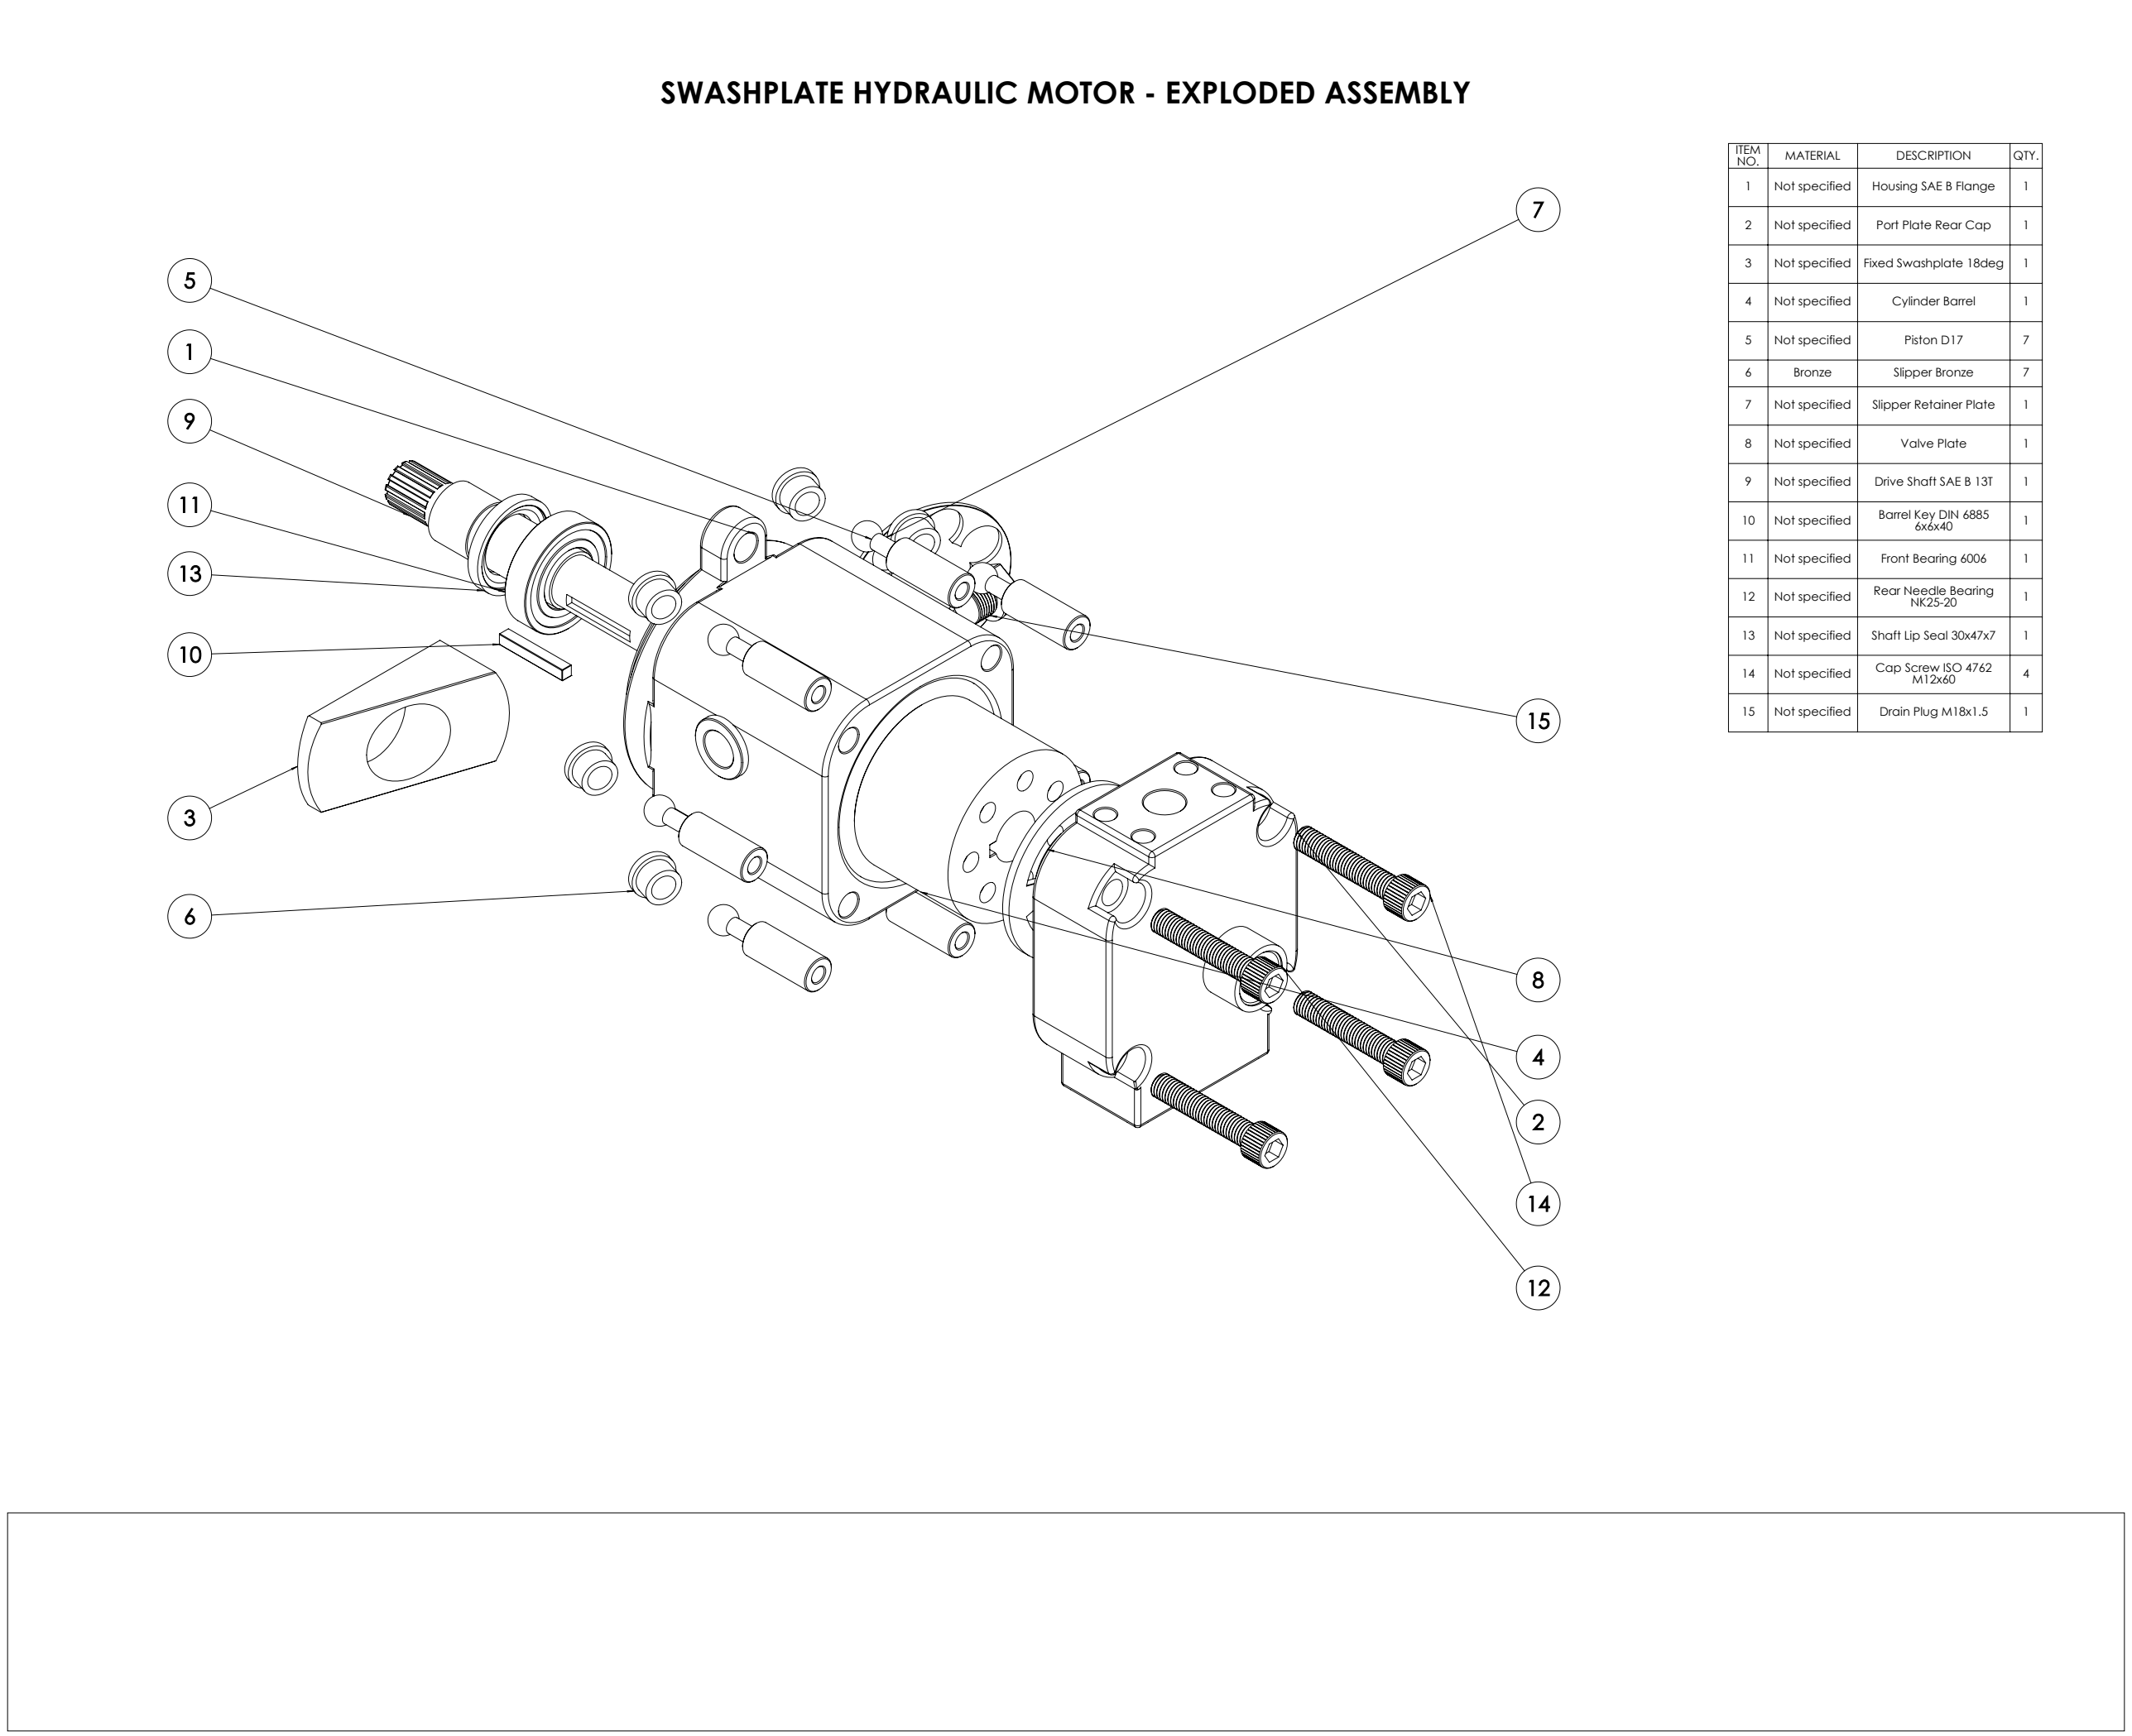
ISO-10303-21;
HEADER;
/* Generated by software containing ST-Developer
 * from STEP Tools, Inc. (www.steptools.com) 
 */

FILE_DESCRIPTION(
/* description */ (''),
/* implementation_level */ '2;1');

FILE_NAME(
/* name */ 'MAS-347',
/* time_stamp */ '2026-10-26T07:49:00-07:00',
/* author */ (''),
/* organization */ (''),
/* preprocessor_version */ 'ST-DEVELOPER v20.2',
/* originating_system */ 'Autodesk Translation Framework v15.15.0.0',
/* authorisation */ '');

FILE_SCHEMA (('AUTOMOTIVE_DESIGN { 1 0 10303 214 3 1 1 }'));
ENDSEC;

DATA;
#10=MECHANICAL_DESIGN_GEOMETRIC_PRESENTATION_REPRESENTATION('',(#177,#178,
#179,#180,#181,#182,#183,#184,#185,#186,#187,#188,#189,#190,#191),#38507);
#11=ITEM_DEFINED_TRANSFORMATION($,$,#15253,#16745);
#12=ITEM_DEFINED_TRANSFORMATION($,$,#15494,#16746);
#13=ITEM_DEFINED_TRANSFORMATION($,$,#15799,#16747);
#14=ITEM_DEFINED_TRANSFORMATION($,$,#15825,#16748);
#15=ITEM_DEFINED_TRANSFORMATION($,$,#15901,#16749);
#16=ITEM_DEFINED_TRANSFORMATION($,$,#15950,#16750);
#17=ITEM_DEFINED_TRANSFORMATION($,$,#16152,#16751);
#18=ITEM_DEFINED_TRANSFORMATION($,$,#16171,#16752);
#19=ITEM_DEFINED_TRANSFORMATION($,$,#16204,#16753);
#20=ITEM_DEFINED_TRANSFORMATION($,$,#16229,#16754);
#21=ITEM_DEFINED_TRANSFORMATION($,$,#16254,#16755);
#22=ITEM_DEFINED_TRANSFORMATION($,$,#16279,#16756);
#23=ITEM_DEFINED_TRANSFORMATION($,$,#16254,#16757);
#24=ITEM_DEFINED_TRANSFORMATION($,$,#16279,#16758);
#25=ITEM_DEFINED_TRANSFORMATION($,$,#16254,#16759);
#26=ITEM_DEFINED_TRANSFORMATION($,$,#16279,#16760);
#27=ITEM_DEFINED_TRANSFORMATION($,$,#16254,#16761);
#28=ITEM_DEFINED_TRANSFORMATION($,$,#16279,#16762);
#29=ITEM_DEFINED_TRANSFORMATION($,$,#16254,#16763);
#30=ITEM_DEFINED_TRANSFORMATION($,$,#16279,#16764);
#31=ITEM_DEFINED_TRANSFORMATION($,$,#16254,#16765);
#32=ITEM_DEFINED_TRANSFORMATION($,$,#16279,#16766);
#33=ITEM_DEFINED_TRANSFORMATION($,$,#16254,#16767);
#34=ITEM_DEFINED_TRANSFORMATION($,$,#16279,#16768);
#35=ITEM_DEFINED_TRANSFORMATION($,$,#16304,#16769);
#36=ITEM_DEFINED_TRANSFORMATION($,$,#16357,#16770);
#37=ITEM_DEFINED_TRANSFORMATION($,$,#16357,#16771);
#38=ITEM_DEFINED_TRANSFORMATION($,$,#16357,#16772);
#39=ITEM_DEFINED_TRANSFORMATION($,$,#16357,#16773);
#40=ITEM_DEFINED_TRANSFORMATION($,$,#16670,#16774);
#41=(
REPRESENTATION_RELATIONSHIP($,$,#38575,#38574)
REPRESENTATION_RELATIONSHIP_WITH_TRANSFORMATION(#11)
SHAPE_REPRESENTATION_RELATIONSHIP()
);
#42=(
REPRESENTATION_RELATIONSHIP($,$,#38576,#38574)
REPRESENTATION_RELATIONSHIP_WITH_TRANSFORMATION(#12)
SHAPE_REPRESENTATION_RELATIONSHIP()
);
#43=(
REPRESENTATION_RELATIONSHIP($,$,#38577,#38574)
REPRESENTATION_RELATIONSHIP_WITH_TRANSFORMATION(#13)
SHAPE_REPRESENTATION_RELATIONSHIP()
);
#44=(
REPRESENTATION_RELATIONSHIP($,$,#38578,#38574)
REPRESENTATION_RELATIONSHIP_WITH_TRANSFORMATION(#14)
SHAPE_REPRESENTATION_RELATIONSHIP()
);
#45=(
REPRESENTATION_RELATIONSHIP($,$,#38579,#38574)
REPRESENTATION_RELATIONSHIP_WITH_TRANSFORMATION(#15)
SHAPE_REPRESENTATION_RELATIONSHIP()
);
#46=(
REPRESENTATION_RELATIONSHIP($,$,#38580,#38574)
REPRESENTATION_RELATIONSHIP_WITH_TRANSFORMATION(#16)
SHAPE_REPRESENTATION_RELATIONSHIP()
);
#47=(
REPRESENTATION_RELATIONSHIP($,$,#38581,#38574)
REPRESENTATION_RELATIONSHIP_WITH_TRANSFORMATION(#17)
SHAPE_REPRESENTATION_RELATIONSHIP()
);
#48=(
REPRESENTATION_RELATIONSHIP($,$,#38582,#38574)
REPRESENTATION_RELATIONSHIP_WITH_TRANSFORMATION(#18)
SHAPE_REPRESENTATION_RELATIONSHIP()
);
#49=(
REPRESENTATION_RELATIONSHIP($,$,#38583,#38574)
REPRESENTATION_RELATIONSHIP_WITH_TRANSFORMATION(#19)
SHAPE_REPRESENTATION_RELATIONSHIP()
);
#50=(
REPRESENTATION_RELATIONSHIP($,$,#38584,#38574)
REPRESENTATION_RELATIONSHIP_WITH_TRANSFORMATION(#20)
SHAPE_REPRESENTATION_RELATIONSHIP()
);
#51=(
REPRESENTATION_RELATIONSHIP($,$,#38585,#38574)
REPRESENTATION_RELATIONSHIP_WITH_TRANSFORMATION(#21)
SHAPE_REPRESENTATION_RELATIONSHIP()
);
#52=(
REPRESENTATION_RELATIONSHIP($,$,#38586,#38574)
REPRESENTATION_RELATIONSHIP_WITH_TRANSFORMATION(#22)
SHAPE_REPRESENTATION_RELATIONSHIP()
);
#53=(
REPRESENTATION_RELATIONSHIP($,$,#38585,#38574)
REPRESENTATION_RELATIONSHIP_WITH_TRANSFORMATION(#23)
SHAPE_REPRESENTATION_RELATIONSHIP()
);
#54=(
REPRESENTATION_RELATIONSHIP($,$,#38586,#38574)
REPRESENTATION_RELATIONSHIP_WITH_TRANSFORMATION(#24)
SHAPE_REPRESENTATION_RELATIONSHIP()
);
#55=(
REPRESENTATION_RELATIONSHIP($,$,#38585,#38574)
REPRESENTATION_RELATIONSHIP_WITH_TRANSFORMATION(#25)
SHAPE_REPRESENTATION_RELATIONSHIP()
);
#56=(
REPRESENTATION_RELATIONSHIP($,$,#38586,#38574)
REPRESENTATION_RELATIONSHIP_WITH_TRANSFORMATION(#26)
SHAPE_REPRESENTATION_RELATIONSHIP()
);
#57=(
REPRESENTATION_RELATIONSHIP($,$,#38585,#38574)
REPRESENTATION_RELATIONSHIP_WITH_TRANSFORMATION(#27)
SHAPE_REPRESENTATION_RELATIONSHIP()
);
#58=(
REPRESENTATION_RELATIONSHIP($,$,#38586,#38574)
REPRESENTATION_RELATIONSHIP_WITH_TRANSFORMATION(#28)
SHAPE_REPRESENTATION_RELATIONSHIP()
);
#59=(
REPRESENTATION_RELATIONSHIP($,$,#38585,#38574)
REPRESENTATION_RELATIONSHIP_WITH_TRANSFORMATION(#29)
SHAPE_REPRESENTATION_RELATIONSHIP()
);
#60=(
REPRESENTATION_RELATIONSHIP($,$,#38586,#38574)
REPRESENTATION_RELATIONSHIP_WITH_TRANSFORMATION(#30)
SHAPE_REPRESENTATION_RELATIONSHIP()
);
#61=(
REPRESENTATION_RELATIONSHIP($,$,#38585,#38574)
REPRESENTATION_RELATIONSHIP_WITH_TRANSFORMATION(#31)
SHAPE_REPRESENTATION_RELATIONSHIP()
);
#62=(
REPRESENTATION_RELATIONSHIP($,$,#38586,#38574)
REPRESENTATION_RELATIONSHIP_WITH_TRANSFORMATION(#32)
SHAPE_REPRESENTATION_RELATIONSHIP()
);
#63=(
REPRESENTATION_RELATIONSHIP($,$,#38585,#38574)
REPRESENTATION_RELATIONSHIP_WITH_TRANSFORMATION(#33)
SHAPE_REPRESENTATION_RELATIONSHIP()
);
#64=(
REPRESENTATION_RELATIONSHIP($,$,#38586,#38574)
REPRESENTATION_RELATIONSHIP_WITH_TRANSFORMATION(#34)
SHAPE_REPRESENTATION_RELATIONSHIP()
);
#65=(
REPRESENTATION_RELATIONSHIP($,$,#38587,#38574)
REPRESENTATION_RELATIONSHIP_WITH_TRANSFORMATION(#35)
SHAPE_REPRESENTATION_RELATIONSHIP()
);
#66=(
REPRESENTATION_RELATIONSHIP($,$,#38588,#38574)
REPRESENTATION_RELATIONSHIP_WITH_TRANSFORMATION(#36)
SHAPE_REPRESENTATION_RELATIONSHIP()
);
#67=(
REPRESENTATION_RELATIONSHIP($,$,#38588,#38574)
REPRESENTATION_RELATIONSHIP_WITH_TRANSFORMATION(#37)
SHAPE_REPRESENTATION_RELATIONSHIP()
);
#68=(
REPRESENTATION_RELATIONSHIP($,$,#38588,#38574)
REPRESENTATION_RELATIONSHIP_WITH_TRANSFORMATION(#38)
SHAPE_REPRESENTATION_RELATIONSHIP()
);
#69=(
REPRESENTATION_RELATIONSHIP($,$,#38588,#38574)
REPRESENTATION_RELATIONSHIP_WITH_TRANSFORMATION(#39)
SHAPE_REPRESENTATION_RELATIONSHIP()
);
#70=(
REPRESENTATION_RELATIONSHIP($,$,#38589,#38574)
REPRESENTATION_RELATIONSHIP_WITH_TRANSFORMATION(#40)
SHAPE_REPRESENTATION_RELATIONSHIP()
);
#71=CONTEXT_DEPENDENT_SHAPE_REPRESENTATION(#41,#38544);
#72=CONTEXT_DEPENDENT_SHAPE_REPRESENTATION(#42,#38545);
#73=CONTEXT_DEPENDENT_SHAPE_REPRESENTATION(#43,#38546);
#74=CONTEXT_DEPENDENT_SHAPE_REPRESENTATION(#44,#38547);
#75=CONTEXT_DEPENDENT_SHAPE_REPRESENTATION(#45,#38548);
#76=CONTEXT_DEPENDENT_SHAPE_REPRESENTATION(#46,#38549);
#77=CONTEXT_DEPENDENT_SHAPE_REPRESENTATION(#47,#38550);
#78=CONTEXT_DEPENDENT_SHAPE_REPRESENTATION(#48,#38551);
#79=CONTEXT_DEPENDENT_SHAPE_REPRESENTATION(#49,#38552);
#80=CONTEXT_DEPENDENT_SHAPE_REPRESENTATION(#50,#38553);
#81=CONTEXT_DEPENDENT_SHAPE_REPRESENTATION(#51,#38554);
#82=CONTEXT_DEPENDENT_SHAPE_REPRESENTATION(#52,#38555);
#83=CONTEXT_DEPENDENT_SHAPE_REPRESENTATION(#53,#38556);
#84=CONTEXT_DEPENDENT_SHAPE_REPRESENTATION(#54,#38557);
#85=CONTEXT_DEPENDENT_SHAPE_REPRESENTATION(#55,#38558);
#86=CONTEXT_DEPENDENT_SHAPE_REPRESENTATION(#56,#38559);
#87=CONTEXT_DEPENDENT_SHAPE_REPRESENTATION(#57,#38560);
#88=CONTEXT_DEPENDENT_SHAPE_REPRESENTATION(#58,#38561);
#89=CONTEXT_DEPENDENT_SHAPE_REPRESENTATION(#59,#38562);
#90=CONTEXT_DEPENDENT_SHAPE_REPRESENTATION(#60,#38563);
#91=CONTEXT_DEPENDENT_SHAPE_REPRESENTATION(#61,#38564);
#92=CONTEXT_DEPENDENT_SHAPE_REPRESENTATION(#62,#38565);
#93=CONTEXT_DEPENDENT_SHAPE_REPRESENTATION(#63,#38566);
#94=CONTEXT_DEPENDENT_SHAPE_REPRESENTATION(#64,#38567);
#95=CONTEXT_DEPENDENT_SHAPE_REPRESENTATION(#65,#38568);
#96=CONTEXT_DEPENDENT_SHAPE_REPRESENTATION(#66,#38569);
#97=CONTEXT_DEPENDENT_SHAPE_REPRESENTATION(#67,#38570);
#98=CONTEXT_DEPENDENT_SHAPE_REPRESENTATION(#68,#38571);
#99=CONTEXT_DEPENDENT_SHAPE_REPRESENTATION(#69,#38572);
#100=CONTEXT_DEPENDENT_SHAPE_REPRESENTATION(#70,#38573);
#101=NEXT_ASSEMBLY_USAGE_OCCURRENCE('01_Housing_SAE_B_Flange:2',
'01_Housing_SAE_B_Flange:2','01_Housing_SAE_B_Flange:2',#38591,#38592,
'01_Housing_SAE_B_Flange:2');
#102=NEXT_ASSEMBLY_USAGE_OCCURRENCE('02_Port_Plate_Rear_Cap:2',
'02_Port_Plate_Rear_Cap:2','02_Port_Plate_Rear_Cap:2',#38591,#38593,
'02_Port_Plate_Rear_Cap:2');
#103=NEXT_ASSEMBLY_USAGE_OCCURRENCE('03_Fixed_Swashplate_18deg:2',
'03_Fixed_Swashplate_18deg:2','03_Fixed_Swashplate_18deg:2',#38591,#38594,
'03_Fixed_Swashplate_18deg:2');
#104=NEXT_ASSEMBLY_USAGE_OCCURRENCE('04_Cylinder_Barrel:2',
'04_Cylinder_Barrel:2','04_Cylinder_Barrel:2',#38591,#38595,
'04_Cylinder_Barrel:2');
#105=NEXT_ASSEMBLY_USAGE_OCCURRENCE('08_Valve_Plate:2',
'08_Valve_Plate:2','08_Valve_Plate:2',#38591,#38596,'08_Valve_Plate:2');
#106=NEXT_ASSEMBLY_USAGE_OCCURRENCE('09_Drive_Shaft_SAE_B_13T:2',
'09_Drive_Shaft_SAE_B_13T:2','09_Drive_Shaft_SAE_B_13T:2',#38591,#38597,
'09_Drive_Shaft_SAE_B_13T:2');
#107=NEXT_ASSEMBLY_USAGE_OCCURRENCE('10_Barrel_Key_DIN_6885_6x6x40:2',
'10_Barrel_Key_DIN_6885_6x6x40:2','10_Barrel_Key_DIN_6885_6x6x40:2',#38591,
#38598,'10_Barrel_Key_DIN_6885_6x6x40:2');
#108=NEXT_ASSEMBLY_USAGE_OCCURRENCE('11_Front_Bearing_6006:2',
'11_Front_Bearing_6006:2','11_Front_Bearing_6006:2',#38591,#38599,
'11_Front_Bearing_6006:2');
#109=NEXT_ASSEMBLY_USAGE_OCCURRENCE('12_Rear_Needle_Bearing_NK25-20:2',
'12_Rear_Needle_Bearing_NK25-20:2','12_Rear_Needle_Bearing_NK25-20:2',#38591,
#38600,'12_Rear_Needle_Bearing_NK25-20:2');
#110=NEXT_ASSEMBLY_USAGE_OCCURRENCE('13_Shaft_Lip_Seal_30x47x7:2',
'13_Shaft_Lip_Seal_30x47x7:2','13_Shaft_Lip_Seal_30x47x7:2',#38591,#38601,
'13_Shaft_Lip_Seal_30x47x7:2');
#111=NEXT_ASSEMBLY_USAGE_OCCURRENCE('05_Piston_D17:2','05_Piston_D17:2',
'05_Piston_D17:2',#38591,#38602,'05_Piston_D17:2');
#112=NEXT_ASSEMBLY_USAGE_OCCURRENCE('06_Slipper_Bronze:2',
'06_Slipper_Bronze:2','06_Slipper_Bronze:2',#38591,#38603,
'06_Slipper_Bronze:2');
#113=NEXT_ASSEMBLY_USAGE_OCCURRENCE('05_Piston_D17:3','05_Piston_D17:3',
'05_Piston_D17:3',#38591,#38602,'05_Piston_D17:3');
#114=NEXT_ASSEMBLY_USAGE_OCCURRENCE('06_Slipper_Bronze:3',
'06_Slipper_Bronze:3','06_Slipper_Bronze:3',#38591,#38603,
'06_Slipper_Bronze:3');
#115=NEXT_ASSEMBLY_USAGE_OCCURRENCE('05_Piston_D17:4','05_Piston_D17:4',
'05_Piston_D17:4',#38591,#38602,'05_Piston_D17:4');
#116=NEXT_ASSEMBLY_USAGE_OCCURRENCE('06_Slipper_Bronze:4',
'06_Slipper_Bronze:4','06_Slipper_Bronze:4',#38591,#38603,
'06_Slipper_Bronze:4');
#117=NEXT_ASSEMBLY_USAGE_OCCURRENCE('05_Piston_D17:5','05_Piston_D17:5',
'05_Piston_D17:5',#38591,#38602,'05_Piston_D17:5');
#118=NEXT_ASSEMBLY_USAGE_OCCURRENCE('06_Slipper_Bronze:5',
'06_Slipper_Bronze:5','06_Slipper_Bronze:5',#38591,#38603,
'06_Slipper_Bronze:5');
#119=NEXT_ASSEMBLY_USAGE_OCCURRENCE('05_Piston_D17:6','05_Piston_D17:6',
'05_Piston_D17:6',#38591,#38602,'05_Piston_D17:6');
#120=NEXT_ASSEMBLY_USAGE_OCCURRENCE('06_Slipper_Bronze:6',
'06_Slipper_Bronze:6','06_Slipper_Bronze:6',#38591,#38603,
'06_Slipper_Bronze:6');
#121=NEXT_ASSEMBLY_USAGE_OCCURRENCE('05_Piston_D17:7','05_Piston_D17:7',
'05_Piston_D17:7',#38591,#38602,'05_Piston_D17:7');
#122=NEXT_ASSEMBLY_USAGE_OCCURRENCE('06_Slipper_Bronze:7',
'06_Slipper_Bronze:7','06_Slipper_Bronze:7',#38591,#38603,
'06_Slipper_Bronze:7');
#123=NEXT_ASSEMBLY_USAGE_OCCURRENCE('05_Piston_D17:8','05_Piston_D17:8',
'05_Piston_D17:8',#38591,#38602,'05_Piston_D17:8');
#124=NEXT_ASSEMBLY_USAGE_OCCURRENCE('06_Slipper_Bronze:8',
'06_Slipper_Bronze:8','06_Slipper_Bronze:8',#38591,#38603,
'06_Slipper_Bronze:8');
#125=NEXT_ASSEMBLY_USAGE_OCCURRENCE('07_Slipper_Retainer_Plate:2',
'07_Slipper_Retainer_Plate:2','07_Slipper_Retainer_Plate:2',#38591,#38604,
'07_Slipper_Retainer_Plate:2');
#126=NEXT_ASSEMBLY_USAGE_OCCURRENCE('14_Cap_Screw_ISO_4762_M12x60:2',
'14_Cap_Screw_ISO_4762_M12x60:2','14_Cap_Screw_ISO_4762_M12x60:2',#38591,
#38605,'14_Cap_Screw_ISO_4762_M12x60:2');
#127=NEXT_ASSEMBLY_USAGE_OCCURRENCE('14_Cap_Screw_ISO_4762_M12x60:3',
'14_Cap_Screw_ISO_4762_M12x60:3','14_Cap_Screw_ISO_4762_M12x60:3',#38591,
#38605,'14_Cap_Screw_ISO_4762_M12x60:3');
#128=NEXT_ASSEMBLY_USAGE_OCCURRENCE('14_Cap_Screw_ISO_4762_M12x60:4',
'14_Cap_Screw_ISO_4762_M12x60:4','14_Cap_Screw_ISO_4762_M12x60:4',#38591,
#38605,'14_Cap_Screw_ISO_4762_M12x60:4');
#129=NEXT_ASSEMBLY_USAGE_OCCURRENCE('14_Cap_Screw_ISO_4762_M12x60:5',
'14_Cap_Screw_ISO_4762_M12x60:5','14_Cap_Screw_ISO_4762_M12x60:5',#38591,
#38605,'14_Cap_Screw_ISO_4762_M12x60:5');
#130=NEXT_ASSEMBLY_USAGE_OCCURRENCE('15_Drain_Plug_M18x1.5:2',
'15_Drain_Plug_M18x1.5:2','15_Drain_Plug_M18x1.5:2',#38591,#38606,
'15_Drain_Plug_M18x1.5:2');
#131=(
BOUNDED_SURFACE()
B_SPLINE_SURFACE(2,2,((#27036,#27037,#27038,#27039,#27040,#27041,#27042,
#27043,#27044),(#27045,#27046,#27047,#27048,#27049,#27050,#27051,#27052,
#27053),(#27054,#27055,#27056,#27057,#27058,#27059,#27060,#27061,#27062),
(#27063,#27064,#27065,#27066,#27067,#27068,#27069,#27070,#27071),(#27072,
#27073,#27074,#27075,#27076,#27077,#27078,#27079,#27080)),.UNSPECIFIED.,
 .F.,.T.,.F.)
B_SPLINE_SURFACE_WITH_KNOTS((3,2,3),(3,2,2,2,3),(-1.42752879197468,-0.232447556257835,
0.962633679459007),(-3.14159265358979,-1.5707963267949,0.,1.5707963267949,
3.14159265358979),.UNSPECIFIED.)
GEOMETRIC_REPRESENTATION_ITEM()
RATIONAL_B_SPLINE_SURFACE(((1.,0.707106781186548,1.,0.707106781186548,1.,
0.707106781186548,1.,0.707106781186548,1.),(0.826721789080264,0.584580583213329,
0.826721789080264,0.584580583213329,0.826721789080264,0.584580583213329,
0.826721789080264,0.584580583213329,0.826721789080264),(1.,0.707106781186548,
1.,0.707106781186548,1.,0.707106781186548,1.,0.707106781186548,1.),(0.826721789080262,
0.584580583213328,0.826721789080262,0.584580583213328,0.826721789080262,
0.584580583213328,0.826721789080262,0.584580583213328,0.826721789080262),
(1.,0.707106781186548,1.,0.707106781186548,1.,0.707106781186548,1.,0.707106781186548,
1.)))
REPRESENTATION_ITEM('')
SURFACE()
);
#132=SPHERICAL_SURFACE('',#15608,1.99999999999999);
#133=SPHERICAL_SURFACE('',#15617,2.);
#134=SPHERICAL_SURFACE('',#15621,2.);
#135=SPHERICAL_SURFACE('',#15628,2.);
#136=SPHERICAL_SURFACE('',#15630,2.);
#137=SPHERICAL_SURFACE('',#15636,2.);
#138=SPHERICAL_SURFACE('',#15638,2.);
#139=SPHERICAL_SURFACE('',#15719,2.);
#140=SPHERICAL_SURFACE('',#15722,2.);
#141=SPHERICAL_SURFACE('',#15737,2.);
#142=SPHERICAL_SURFACE('',#15745,1.99999999999999);
#143=SPHERICAL_SURFACE('',#15749,1.99999999999999);
#144=SPHERICAL_SURFACE('',#15753,1.99999999999999);
#145=SPHERICAL_SURFACE('',#15769,1.99999999999999);
#146=SPHERICAL_SURFACE('',#16295,7.02);
#147=SHAPE_REPRESENTATION_RELATIONSHIP('SRR','None',#38575,#162);
#148=SHAPE_REPRESENTATION_RELATIONSHIP('SRR','None',#38576,#163);
#149=SHAPE_REPRESENTATION_RELATIONSHIP('SRR','None',#38577,#164);
#150=SHAPE_REPRESENTATION_RELATIONSHIP('SRR','None',#38578,#165);
#151=SHAPE_REPRESENTATION_RELATIONSHIP('SRR','None',#38579,#166);
#152=SHAPE_REPRESENTATION_RELATIONSHIP('SRR','None',#38580,#167);
#153=SHAPE_REPRESENTATION_RELATIONSHIP('SRR','None',#38581,#168);
#154=SHAPE_REPRESENTATION_RELATIONSHIP('SRR','None',#38582,#169);
#155=SHAPE_REPRESENTATION_RELATIONSHIP('SRR','None',#38583,#170);
#156=SHAPE_REPRESENTATION_RELATIONSHIP('SRR','None',#38584,#171);
#157=SHAPE_REPRESENTATION_RELATIONSHIP('SRR','None',#38585,#172);
#158=SHAPE_REPRESENTATION_RELATIONSHIP('SRR','None',#38586,#173);
#159=SHAPE_REPRESENTATION_RELATIONSHIP('SRR','None',#38587,#174);
#160=SHAPE_REPRESENTATION_RELATIONSHIP('SRR','None',#38588,#175);
#161=SHAPE_REPRESENTATION_RELATIONSHIP('SRR','None',#38589,#176);
#162=ADVANCED_BREP_SHAPE_REPRESENTATION('',(#192),#38492);
#163=ADVANCED_BREP_SHAPE_REPRESENTATION('',(#193),#38493);
#164=ADVANCED_BREP_SHAPE_REPRESENTATION('',(#194),#38494);
#165=ADVANCED_BREP_SHAPE_REPRESENTATION('',(#195),#38495);
#166=ADVANCED_BREP_SHAPE_REPRESENTATION('',(#196),#38496);
#167=ADVANCED_BREP_SHAPE_REPRESENTATION('',(#197),#38497);
#168=ADVANCED_BREP_SHAPE_REPRESENTATION('',(#198),#38498);
#169=ADVANCED_BREP_SHAPE_REPRESENTATION('',(#199),#38499);
#170=ADVANCED_BREP_SHAPE_REPRESENTATION('',(#200),#38500);
#171=ADVANCED_BREP_SHAPE_REPRESENTATION('',(#201),#38501);
#172=ADVANCED_BREP_SHAPE_REPRESENTATION('',(#202),#38502);
#173=ADVANCED_BREP_SHAPE_REPRESENTATION('',(#203),#38503);
#174=ADVANCED_BREP_SHAPE_REPRESENTATION('',(#204),#38504);
#175=ADVANCED_BREP_SHAPE_REPRESENTATION('',(#205),#38505);
#176=ADVANCED_BREP_SHAPE_REPRESENTATION('',(#206),#38506);
#177=STYLED_ITEM('',(#38699),#192);
#178=STYLED_ITEM('',(#38713),#193);
#179=STYLED_ITEM('',(#38706),#194);
#180=STYLED_ITEM('',(#38734),#195);
#181=STYLED_ITEM('',(#38706),#196);
#182=STYLED_ITEM('',(#38720),#197);
#183=STYLED_ITEM('',(#38720),#198);
#184=STYLED_ITEM('',(#38720),#199);
#185=STYLED_ITEM('',(#38720),#200);
#186=STYLED_ITEM('',(#38727),#201);
#187=STYLED_ITEM('',(#38713),#202);
#188=STYLED_ITEM('',(#38713),#203);
#189=STYLED_ITEM('',(#38713),#204);
#190=STYLED_ITEM('',(#38727),#205);
#191=STYLED_ITEM('',(#38706),#206);
#192=MANIFOLD_SOLID_BREP('Body1',#15071);
#193=MANIFOLD_SOLID_BREP('Body1',#15072);
#194=MANIFOLD_SOLID_BREP('Body1',#15073);
#195=MANIFOLD_SOLID_BREP('Body1',#15074);
#196=MANIFOLD_SOLID_BREP('Body1',#15075);
#197=MANIFOLD_SOLID_BREP('Body1',#15076);
#198=MANIFOLD_SOLID_BREP('Body1',#15077);
#199=MANIFOLD_SOLID_BREP('Body1',#15078);
#200=MANIFOLD_SOLID_BREP('Body1',#15079);
#201=MANIFOLD_SOLID_BREP('Body1',#15080);
#202=MANIFOLD_SOLID_BREP('Body1',#15081);
#203=MANIFOLD_SOLID_BREP('Slipper_Body',#15082);
#204=MANIFOLD_SOLID_BREP('Body1',#15083);
#205=MANIFOLD_SOLID_BREP('Body1',#15084);
#206=MANIFOLD_SOLID_BREP('Body1',#15085);
#207=B_SPLINE_SURFACE_WITH_KNOTS('',3,3,((#22067,#22068,#22069,#22070,#22071,
#22072,#22073),(#22074,#22075,#22076,#22077,#22078,#22079,#22080),(#22081,
#22082,#22083,#22084,#22085,#22086,#22087),(#22088,#22089,#22090,#22091,
#22092,#22093,#22094)),.UNSPECIFIED.,.F.,.F.,.F.,(4,4),(4,1,1,1,4),(0.,
1.),(-0.462000333519479,-0.263998422594088,-0.131997148643828,-0.0329961931811326,
4.1253064325321E-6),.UNSPECIFIED.);
#208=B_SPLINE_SURFACE_WITH_KNOTS('',3,3,((#22108,#22109,#22110,#22111,#22112,
#22113,#22114,#22115,#22116,#22117),(#22118,#22119,#22120,#22121,#22122,
#22123,#22124,#22125,#22126,#22127),(#22128,#22129,#22130,#22131,#22132,
#22133,#22134,#22135,#22136,#22137),(#22138,#22139,#22140,#22141,#22142,
#22143,#22144,#22145,#22146,#22147),(#22148,#22149,#22150,#22151,#22152,
#22153,#22154,#22155,#22156,#22157),(#22158,#22159,#22160,#22161,#22162,
#22163,#22164,#22165,#22166,#22167),(#22168,#22169,#22170,#22171,#22172,
#22173,#22174,#22175,#22176,#22177)),.UNSPECIFIED.,.F.,.F.,.F.,(4,1,1,1,
4),(4,1,1,1,1,1,1,4),(0.,0.285714285714286,0.571428571428571,0.785714285714286,
1.),(-7.35549329570849,-7.06046758790365,-6.76544188009881,-6.47041617229397,
-6.17539046448912,-5.88036475668429,-5.58533904887944,-5.2903133410746),
 .UNSPECIFIED.);
#209=B_SPLINE_SURFACE_WITH_KNOTS('',3,3,((#22179,#22180,#22181,#22182,#22183,
#22184,#22185,#22186,#22187,#22188,#22189,#22190,#22191,#22192,#22193,#22194,
#22195,#22196,#22197,#22198,#22199,#22200,#22201,#22202,#22203),(#22204,
#22205,#22206,#22207,#22208,#22209,#22210,#22211,#22212,#22213,#22214,#22215,
#22216,#22217,#22218,#22219,#22220,#22221,#22222,#22223,#22224,#22225,#22226,
#22227,#22228),(#22229,#22230,#22231,#22232,#22233,#22234,#22235,#22236,
#22237,#22238,#22239,#22240,#22241,#22242,#22243,#22244,#22245,#22246,#22247,
#22248,#22249,#22250,#22251,#22252,#22253),(#22254,#22255,#22256,#22257,
#22258,#22259,#22260,#22261,#22262,#22263,#22264,#22265,#22266,#22267,#22268,
#22269,#22270,#22271,#22272,#22273,#22274,#22275,#22276,#22277,#22278),
(#22279,#22280,#22281,#22282,#22283,#22284,#22285,#22286,#22287,#22288,
#22289,#22290,#22291,#22292,#22293,#22294,#22295,#22296,#22297,#22298,#22299,
#22300,#22301,#22302,#22303)),.UNSPECIFIED.,.F.,.F.,.F.,(4,1,4),(4,2,1,
1,1,1,1,1,1,1,1,1,1,1,1,1,1,1,1,1,1,4),(0.,0.571428571428571,1.),(-0.461724827521327,
-0.461389911948815,-0.455622538049454,-0.449855164150094,-0.438320416351374,
-0.415250920753933,-0.392181425156492,-0.369111929559052,-0.346042433961611,
-0.32297293836417,-0.29990344276673,-0.276833947169289,-0.253764451571848,
-0.230694955974407,-0.207625460376967,-0.196090712578246,-0.184555964779526,
-0.138416973584644,-0.115347477987204,-0.0922779823897629,-0.0461389911948815,
0.),.UNSPECIFIED.);
#210=B_SPLINE_SURFACE_WITH_KNOTS('',3,3,((#22314,#22315,#22316,#22317,#22318,
#22319,#22320,#22321,#22322,#22323),(#22324,#22325,#22326,#22327,#22328,
#22329,#22330,#22331,#22332,#22333),(#22334,#22335,#22336,#22337,#22338,
#22339,#22340,#22341,#22342,#22343),(#22344,#22345,#22346,#22347,#22348,
#22349,#22350,#22351,#22352,#22353),(#22354,#22355,#22356,#22357,#22358,
#22359,#22360,#22361,#22362,#22363),(#22364,#22365,#22366,#22367,#22368,
#22369,#22370,#22371,#22372,#22373)),.UNSPECIFIED.,.F.,.F.,.F.,(4,1,1,4),
(4,1,1,1,1,1,1,4),(0.,0.285714285714286,0.571428571428571,1.),(4.72327004783361,
5.43406096940559,6.14485189097757,6.85564281254955,7.56643373412153,8.27722465569351,
8.98801557726548,9.69880649883746),.UNSPECIFIED.);
#211=B_SPLINE_SURFACE_WITH_KNOTS('',3,3,((#22374,#22375,#22376,#22377,#22378,
#22379),(#22380,#22381,#22382,#22383,#22384,#22385),(#22386,#22387,#22388,
#22389,#22390,#22391),(#22392,#22393,#22394,#22395,#22396,#22397)),
 .UNSPECIFIED.,.F.,.F.,.F.,(4,4),(4,1,1,4),(0.,1.),(-0.461769339103211,
-0.197899101291517,-0.0659639823856703,3.57706725334641E-6),
 .UNSPECIFIED.);
#212=B_SPLINE_SURFACE_WITH_KNOTS('',3,3,((#22412,#22413,#22414,#22415,#22416,
#22417,#22418,#22419,#22420,#22421),(#22422,#22423,#22424,#22425,#22426,
#22427,#22428,#22429,#22430,#22431),(#22432,#22433,#22434,#22435,#22436,
#22437,#22438,#22439,#22440,#22441),(#22442,#22443,#22444,#22445,#22446,
#22447,#22448,#22449,#22450,#22451),(#22452,#22453,#22454,#22455,#22456,
#22457,#22458,#22459,#22460,#22461),(#22462,#22463,#22464,#22465,#22466,
#22467,#22468,#22469,#22470,#22471),(#22472,#22473,#22474,#22475,#22476,
#22477,#22478,#22479,#22480,#22481)),.UNSPECIFIED.,.F.,.F.,.F.,(4,1,1,1,
4),(4,1,1,1,1,1,1,4),(0.,0.285714285714286,0.571428571428571,0.785714285714286,
1.),(-7.35549329570849,-7.06046758790365,-6.76544188009881,-6.47041617229397,
-6.17539046448913,-5.88036475668429,-5.58533904887945,-5.29031334107461),
 .UNSPECIFIED.);
#213=B_SPLINE_SURFACE_WITH_KNOTS('',3,3,((#22485,#22486,#22487,#22488,#22489,
#22490),(#22491,#22492,#22493,#22494,#22495,#22496),(#22497,#22498,#22499,
#22500,#22501,#22502),(#22503,#22504,#22505,#22506,#22507,#22508)),
 .UNSPECIFIED.,.F.,.F.,.F.,(4,4),(4,1,1,4),(0.,1.),(-0.461725499841195,
-0.395764714149595,-0.263843142766397,0.),.UNSPECIFIED.);
#214=B_SPLINE_SURFACE_WITH_KNOTS('',3,3,((#22519,#22520,#22521,#22522,#22523,
#22524,#22525,#22526,#22527,#22528),(#22529,#22530,#22531,#22532,#22533,
#22534,#22535,#22536,#22537,#22538),(#22539,#22540,#22541,#22542,#22543,
#22544,#22545,#22546,#22547,#22548),(#22549,#22550,#22551,#22552,#22553,
#22554,#22555,#22556,#22557,#22558),(#22559,#22560,#22561,#22562,#22563,
#22564,#22565,#22566,#22567,#22568),(#22569,#22570,#22571,#22572,#22573,
#22574,#22575,#22576,#22577,#22578)),.UNSPECIFIED.,.F.,.F.,.F.,(4,1,1,4),
(4,1,1,1,1,1,1,4),(0.,0.285714285714286,0.571428571428571,1.),(4.72327004804774,
5.43406096961972,6.1448518911917,6.85564281276368,7.56643373433566,8.27722465590764,
8.98801557747962,9.6988064990516),.UNSPECIFIED.);
#215=B_SPLINE_SURFACE_WITH_KNOTS('',3,3,((#22745,#22746,#22747,#22748,#22749,
#22750,#22751,#22752,#22753,#22754,#22755,#22756),(#22757,#22758,#22759,
#22760,#22761,#22762,#22763,#22764,#22765,#22766,#22767,#22768),(#22769,
#22770,#22771,#22772,#22773,#22774,#22775,#22776,#22777,#22778,#22779,#22780),
(#22781,#22782,#22783,#22784,#22785,#22786,#22787,#22788,#22789,#22790,
#22791,#22792)),.UNSPECIFIED.,.F.,.F.,.F.,(4,4),(4,2,2,2,2,4),(0.,1.),(1.10145879772751,
1.32414222732706,1.45197453595802,1.57980684458897,1.70763915321993,1.80249027418853),
 .UNSPECIFIED.);
#216=B_SPLINE_SURFACE_WITH_KNOTS('',3,3,((#22823,#22824,#22825,#22826),
(#22827,#22828,#22829,#22830),(#22831,#22832,#22833,#22834),(#22835,#22836,
#22837,#22838)),.UNSPECIFIED.,.F.,.F.,.F.,(4,4),(4,4),(0.,1.),(-2.26119471261739,
-2.15398534032161),.UNSPECIFIED.);
#217=B_SPLINE_SURFACE_WITH_KNOTS('',3,3,((#22856,#22857,#22858,#22859),
(#22860,#22861,#22862,#22863),(#22864,#22865,#22866,#22867),(#22868,#22869,
#22870,#22871)),.UNSPECIFIED.,.F.,.F.,.F.,(4,4),(4,4),(0.,1.),(-0.987607313268187,
-0.880397940972402),.UNSPECIFIED.);
#218=B_SPLINE_SURFACE_WITH_KNOTS('',3,3,((#22880,#22881,#22882,#22883,#22884,
#22885,#22886,#22887),(#22888,#22889,#22890,#22891,#22892,#22893,#22894,
#22895),(#22896,#22897,#22898,#22899,#22900,#22901,#22902,#22903),(#22904,
#22905,#22906,#22907,#22908,#22909,#22910,#22911)),.UNSPECIFIED.,.F.,.F.,
 .F.,(4,4),(4,1,1,2,4),(0.,1.),(2.51916325679745,2.63563179243579,2.86856886371248,
3.10150593498916,3.18038929530694),.UNSPECIFIED.);
#219=B_SPLINE_SURFACE_WITH_KNOTS('',3,3,((#22934,#22935,#22936,#22937),
(#22938,#22939,#22940,#22941),(#22942,#22943,#22944,#22945),(#22946,#22947,
#22948,#22949)),.UNSPECIFIED.,.F.,.F.,.F.,(4,4),(4,4),(0.,1.),(-0.666064399610344,
-0.552453261527181),.UNSPECIFIED.);
#220=B_SPLINE_SURFACE_WITH_KNOTS('',3,3,((#22958,#22959,#22960,#22961),
(#22962,#22963,#22964,#22965),(#22966,#22967,#22968,#22969),(#22970,#22971,
#22972,#22973)),.UNSPECIFIED.,.F.,.F.,.F.,(4,4),(4,4),(0.,1.),(-5.7307320456524,
-5.61712090756923),.UNSPECIFIED.);
#221=B_SPLINE_SURFACE_WITH_KNOTS('',3,3,((#23021,#23022,#23023,#23024,#23025,
#23026,#23027,#23028,#23029,#23030,#23031,#23032),(#23033,#23034,#23035,
#23036,#23037,#23038,#23039,#23040,#23041,#23042,#23043,#23044),(#23045,
#23046,#23047,#23048,#23049,#23050,#23051,#23052,#23053,#23054,#23055,#23056),
(#23057,#23058,#23059,#23060,#23061,#23062,#23063,#23064,#23065,#23066,
#23067,#23068)),.UNSPECIFIED.,.F.,.F.,.F.,(4,4),(4,1,1,1,1,1,1,2,4),(0.,
1.),(1.17201798267167,1.354117347086,1.53621671150032,1.62726639370748,
1.67279123481106,1.71831607591465,1.90041544032897,2.08251480474329,2.14666332293336),
 .UNSPECIFIED.);
#222=B_SPLINE_SURFACE_WITH_KNOTS('',3,3,((#23104,#23105,#23106,#23107),
(#23108,#23109,#23110,#23111),(#23112,#23113,#23114,#23115),(#23116,#23117,
#23118,#23119)),.UNSPECIFIED.,.F.,.F.,.F.,(4,4),(4,4),(0.,1.),(2.29711532831763,
2.37317063593509),.UNSPECIFIED.);
#223=B_SPLINE_SURFACE_WITH_KNOTS('',3,3,((#23137,#23138,#23139,#23140),
(#23141,#23142,#23143,#23144),(#23145,#23146,#23147,#23148),(#23149,#23150,
#23151,#23152)),.UNSPECIFIED.,.F.,.F.,.F.,(4,4),(4,4),(0.,1.),(-2.37317063593509,
-2.29711532831763),.UNSPECIFIED.);
#224=B_SPLINE_SURFACE_WITH_KNOTS('',3,3,((#23161,#23162,#23163,#23164,#23165,
#23166,#23167,#23168),(#23169,#23170,#23171,#23172,#23173,#23174,#23175,
#23176),(#23177,#23178,#23179,#23180,#23181,#23182,#23183,#23184),(#23185,
#23186,#23187,#23188,#23189,#23190,#23191,#23192)),.UNSPECIFIED.,.F.,.F.,
 .F.,(4,4),(4,1,1,2,4),(0.,1.),(1.10145879772751,1.34393093992448,1.46516701102296,
1.70763915321993,1.80249027418852),.UNSPECIFIED.);
#225=B_SPLINE_SURFACE_WITH_KNOTS('',3,3,((#23215,#23216,#23217,#23218),
(#23219,#23220,#23221,#23222),(#23223,#23224,#23225,#23226),(#23227,#23228,
#23229,#23230)),.UNSPECIFIED.,.F.,.F.,.F.,(4,4),(4,4),(0.,1.),(-2.26119471261739,
-2.1539853403216),.UNSPECIFIED.);
#226=B_SPLINE_SURFACE_WITH_KNOTS('',3,3,((#23239,#23240,#23241,#23242),
(#23243,#23244,#23245,#23246),(#23247,#23248,#23249,#23250),(#23251,#23252,
#23253,#23254)),.UNSPECIFIED.,.F.,.F.,.F.,(4,4),(4,4),(0.,1.),(-0.987607313268191,
-0.880397940972402),.UNSPECIFIED.);
#227=B_SPLINE_SURFACE_WITH_KNOTS('',3,3,((#23285,#23286,#23287,#23288,#23289,
#23290,#23291,#23292,#23293,#23294),(#23295,#23296,#23297,#23298,#23299,
#23300,#23301,#23302,#23303,#23304),(#23305,#23306,#23307,#23308,#23309,
#23310,#23311,#23312,#23313,#23314),(#23315,#23316,#23317,#23318,#23319,
#23320,#23321,#23322,#23323,#23324)),.UNSPECIFIED.,.F.,.F.,.F.,(4,4),(4,
2,1,1,1,1,4),(0.,1.),(2.55343333368553,2.64828445465413,2.76952052575261,
2.89075659685109,3.01199266794958,3.07261070349882,3.25446481014654),
 .UNSPECIFIED.);
#228=B_SPLINE_SURFACE_WITH_KNOTS('',3,3,((#23351,#23352,#23353,#23354),
(#23355,#23356,#23357,#23358),(#23359,#23360,#23361,#23362),(#23363,#23364,
#23365,#23366)),.UNSPECIFIED.,.F.,.F.,.F.,(4,4),(4,4),(0.,1.),(-5.40278736620718,
-5.29557799391139),.UNSPECIFIED.);
#229=B_SPLINE_SURFACE_WITH_KNOTS('',3,3,((#23383,#23384,#23385,#23386),
(#23387,#23388,#23389,#23390),(#23391,#23392,#23393,#23394),(#23395,#23396,
#23397,#23398)),.UNSPECIFIED.,.F.,.F.,.F.,(4,4),(4,4),(0.,1.),(-4.12919996685799,
-4.0219905945622),.UNSPECIFIED.);
#230=B_SPLINE_SURFACE_WITH_KNOTS('',3,3,((#23407,#23408,#23409,#23410,#23411,
#23412),(#23413,#23414,#23415,#23416,#23417,#23418),(#23419,#23420,#23421,
#23422,#23423,#23424),(#23425,#23426,#23427,#23428,#23429,#23430)),
 .UNSPECIFIED.,.F.,.F.,.F.,(4,4),(4,1,1,4),(0.,1.),(2.51916325679745,2.70808498208588,
2.8970067073743,3.18038929530694),.UNSPECIFIED.);
#231=B_SPLINE_SURFACE_WITH_KNOTS('',3,3,((#23441,#23442,#23443,#23444),
(#23445,#23446,#23447,#23448),(#23449,#23450,#23451,#23452),(#23453,#23454,
#23455,#23456)),.UNSPECIFIED.,.F.,.F.,.F.,(4,4),(4,4),(0.,1.),(-0.666064399610344,
-0.552453261527181),.UNSPECIFIED.);
#232=B_SPLINE_SURFACE_WITH_KNOTS('',3,3,((#23461,#23462,#23463,#23464),
(#23465,#23466,#23467,#23468),(#23469,#23470,#23471,#23472),(#23473,#23474,
#23475,#23476)),.UNSPECIFIED.,.F.,.F.,.F.,(4,4),(4,4),(0.,1.),(-5.7307320456524,
-5.61712090756924),.UNSPECIFIED.);
#233=B_SPLINE_SURFACE_WITH_KNOTS('',3,3,((#23491,#23492,#23493,#23494,#23495,
#23496),(#23497,#23498,#23499,#23500,#23501,#23502),(#23503,#23504,#23505,
#23506,#23507,#23508),(#23509,#23510,#23511,#23512,#23513,#23514)),
 .UNSPECIFIED.,.F.,.F.,.F.,(4,4),(4,1,1,4),(0.,1.),(2.55343333368552,2.85387539502596,
3.05417010258625,3.25446481014654),.UNSPECIFIED.);
#234=B_SPLINE_SURFACE_WITH_KNOTS('',3,3,((#23533,#23534,#23535,#23536),
(#23537,#23538,#23539,#23540),(#23541,#23542,#23543,#23544),(#23545,#23546,
#23547,#23548)),.UNSPECIFIED.,.F.,.F.,.F.,(4,4),(4,4),(0.,1.),(0.880397940972406,
0.987607313268191),.UNSPECIFIED.);
#235=B_SPLINE_SURFACE_WITH_KNOTS('',3,3,((#23566,#23567,#23568,#23569),
(#23570,#23571,#23572,#23573),(#23574,#23575,#23576,#23577),(#23578,#23579,
#23580,#23581)),.UNSPECIFIED.,.F.,.F.,.F.,(4,4),(4,4),(0.,1.),(2.1539853403216,
2.26119471261739),.UNSPECIFIED.);
#236=B_SPLINE_SURFACE_WITH_KNOTS('',3,3,((#23590,#23591,#23592,#23593,#23594,
#23595,#23596,#23597,#23598,#23599,#23600,#23601,#23602),(#23603,#23604,
#23605,#23606,#23607,#23608,#23609,#23610,#23611,#23612,#23613,#23614,#23615),
(#23616,#23617,#23618,#23619,#23620,#23621,#23622,#23623,#23624,#23625,
#23626,#23627,#23628),(#23629,#23630,#23631,#23632,#23633,#23634,#23635,
#23636,#23637,#23638,#23639,#23640,#23641)),.UNSPECIFIED.,.F.,.F.,.F.,(4,
4),(4,2,1,1,1,1,1,2,4),(0.,1.),(1.17201798267168,1.23616650086174,1.37722455150867,
1.51828260215559,1.58881162747905,1.65934065280252,1.80039870344944,1.94145675409637,
2.14666332293336),.UNSPECIFIED.);
#237=B_SPLINE_SURFACE_WITH_KNOTS('',3,3,((#23679,#23680,#23681,#23682),
(#23683,#23684,#23685,#23686),(#23687,#23688,#23689,#23690),(#23691,#23692,
#23693,#23694)),.UNSPECIFIED.,.F.,.F.,.F.,(4,4),(4,4),(0.,1.),(2.29711532831763,
2.37317063593509),.UNSPECIFIED.);
#238=B_SPLINE_SURFACE_WITH_KNOTS('',3,3,((#23703,#23704,#23705,#23706),
(#23707,#23708,#23709,#23710),(#23711,#23712,#23713,#23714),(#23715,#23716,
#23717,#23718)),.UNSPECIFIED.,.F.,.F.,.F.,(4,4),(4,4),(0.,1.),(-2.37317063593509,
-2.29711532831763),.UNSPECIFIED.);
#239=B_SPLINE_SURFACE_WITH_KNOTS('',3,3,((#23741,#23742,#23743,#23744),
(#23745,#23746,#23747,#23748),(#23749,#23750,#23751,#23752),(#23753,#23754,
#23755,#23756)),.UNSPECIFIED.,.F.,.F.,.F.,(4,4),(4,4),(0.,1.),(-0.626198664785115,
-0.624325079343485),.UNSPECIFIED.);
#240=B_SPLINE_SURFACE_WITH_KNOTS('',3,3,((#23777,#23778,#23779,#23780,#23781,
#23782,#23783,#23784,#23785,#23786),(#23787,#23788,#23789,#23790,#23791,
#23792,#23793,#23794,#23795,#23796),(#23797,#23798,#23799,#23800,#23801,
#23802,#23803,#23804,#23805,#23806),(#23807,#23808,#23809,#23810,#23811,
#23812,#23813,#23814,#23815,#23816)),.UNSPECIFIED.,.F.,.F.,.F.,(4,4),(4,
2,2,2,4),(0.,1.),(-0.624325079343485,-0.380129337104056,-0.301935532404242,
-0.237254059228639,-0.209869946944685),.UNSPECIFIED.);
#241=B_SPLINE_SURFACE_WITH_KNOTS('',3,3,((#23843,#23844,#23845,#23846),
(#23847,#23848,#23849,#23850),(#23851,#23852,#23853,#23854),(#23855,#23856,
#23857,#23858)),.UNSPECIFIED.,.F.,.F.,.F.,(4,4),(4,4),(0.,1.),(-0.626730655849168,
-0.626198664785115),.UNSPECIFIED.);
#242=B_SPLINE_SURFACE_WITH_KNOTS('',3,3,((#23898,#23899,#23900,#23901),
(#23902,#23903,#23904,#23905),(#23906,#23907,#23908,#23909),(#23910,#23911,
#23912,#23913)),.UNSPECIFIED.,.F.,.F.,.F.,(4,4),(4,4),(0.,1.),(1.48736624018428,
1.50825556499841),.UNSPECIFIED.);
#243=B_SPLINE_SURFACE_WITH_KNOTS('',3,3,((#23922,#23923,#23924,#23925),
(#23926,#23927,#23928,#23929),(#23930,#23931,#23932,#23933),(#23934,#23935,
#23936,#23937)),.UNSPECIFIED.,.F.,.F.,.F.,(4,4),(4,4),(0.,1.),(0.,1.),
 .UNSPECIFIED.);
#244=B_SPLINE_SURFACE_WITH_KNOTS('',3,3,((#23981,#23982,#23983,#23984,#23985),
(#23986,#23987,#23988,#23989,#23990),(#23991,#23992,#23993,#23994,#23995),
(#23996,#23997,#23998,#23999,#24000)),.UNSPECIFIED.,.F.,.F.,.F.,(4,4),(4,
1,4),(0.,1.),(0.,0.000208214441420064,0.000485833696646816),
 .UNSPECIFIED.);
#245=B_SPLINE_SURFACE_WITH_KNOTS('',3,3,((#24028,#24029,#24030,#24031),
(#24032,#24033,#24034,#24035),(#24036,#24037,#24038,#24039),(#24040,#24041,
#24042,#24043)),.UNSPECIFIED.,.F.,.F.,.F.,(4,4),(4,4),(0.,1.),(-0.00166298225714781,
0.),.UNSPECIFIED.);
#246=B_SPLINE_SURFACE_WITH_KNOTS('',3,3,((#24062,#24063,#24064,#24065,#24066,
#24067,#24068,#24069,#24070,#24071,#24072,#24073),(#24074,#24075,#24076,
#24077,#24078,#24079,#24080,#24081,#24082,#24083,#24084,#24085),(#24086,
#24087,#24088,#24089,#24090,#24091,#24092,#24093,#24094,#24095,#24096,#24097),
(#24098,#24099,#24100,#24101,#24102,#24103,#24104,#24105,#24106,#24107,
#24108,#24109)),.UNSPECIFIED.,.F.,.F.,.F.,(4,4),(4,2,2,2,2,4),(0.,1.),(-0.369530672027591,
-0.345224711421131,-0.287813854984672,-0.218409540651057,-0.120337282444558,
-0.00166298225714781),.UNSPECIFIED.);
#247=B_SPLINE_SURFACE_WITH_KNOTS('',3,3,((#24157,#24158,#24159,#24160),
(#24161,#24162,#24163,#24164),(#24165,#24166,#24167,#24168),(#24169,#24170,
#24171,#24172)),.UNSPECIFIED.,.F.,.F.,.F.,(4,4),(4,4),(0.,1.),(4.77492974218118,
4.7958190669953),.UNSPECIFIED.);
#248=B_SPLINE_SURFACE_WITH_KNOTS('',3,3,((#24181,#24182,#24183,#24184),
(#24185,#24186,#24187,#24188),(#24189,#24190,#24191,#24192),(#24193,#24194,
#24195,#24196)),.UNSPECIFIED.,.F.,.F.,.F.,(4,4),(4,4),(0.,1.),(0.,1.),
 .UNSPECIFIED.);
#249=B_SPLINE_SURFACE_WITH_KNOTS('',3,3,((#24333,#24334,#24335,#24336,#24337,
#24338,#24339,#24340,#24341,#24342,#24343,#24344,#24345,#24346,#24347,#24348,
#24349,#24350,#24351,#24352,#24353,#24354),(#24355,#24356,#24357,#24358,
#24359,#24360,#24361,#24362,#24363,#24364,#24365,#24366,#24367,#24368,#24369,
#24370,#24371,#24372,#24373,#24374,#24375,#24376),(#24377,#24378,#24379,
#24380,#24381,#24382,#24383,#24384,#24385,#24386,#24387,#24388,#24389,#24390,
#24391,#24392,#24393,#24394,#24395,#24396,#24397,#24398),(#24399,#24400,
#24401,#24402,#24403,#24404,#24405,#24406,#24407,#24408,#24409,#24410,#24411,
#24412,#24413,#24414,#24415,#24416,#24417,#24418,#24419,#24420),(#24421,
#24422,#24423,#24424,#24425,#24426,#24427,#24428,#24429,#24430,#24431,#24432,
#24433,#24434,#24435,#24436,#24437,#24438,#24439,#24440,#24441,#24442)),
 .UNSPECIFIED.,.F.,.T.,.F.,(4,1,4),(4,1,1,1,1,1,1,1,1,1,1,1,1,1,1,1,1,1,
1,4),(0.,0.571428571428571,1.),(0.,0.133807235852271,0.267614471704543,
0.535228943409085,0.802843415113627,1.07045788681817,1.2488675346212,1.42727718242423,
1.60568683022725,1.78409647803028,1.96250612583331,2.14091577363634,2.40853024534088,
2.54233748119315,2.67614471704543,2.94375918874997,3.21137366045451,3.47898813215905,
3.61279536801132,3.74660260386359),.UNSPECIFIED.);
#250=B_SPLINE_SURFACE_WITH_KNOTS('',3,3,((#24656,#24657,#24658,#24659,#24660,
#24661,#24662,#24663,#24664,#24665,#24666,#24667,#24668,#24669,#24670,#24671,
#24672,#24673),(#24674,#24675,#24676,#24677,#24678,#24679,#24680,#24681,
#24682,#24683,#24684,#24685,#24686,#24687,#24688,#24689,#24690,#24691),
(#24692,#24693,#24694,#24695,#24696,#24697,#24698,#24699,#24700,#24701,
#24702,#24703,#24704,#24705,#24706,#24707,#24708,#24709),(#24710,#24711,
#24712,#24713,#24714,#24715,#24716,#24717,#24718,#24719,#24720,#24721,#24722,
#24723,#24724,#24725,#24726,#24727),(#24728,#24729,#24730,#24731,#24732,
#24733,#24734,#24735,#24736,#24737,#24738,#24739,#24740,#24741,#24742,#24743,
#24744,#24745),(#24746,#24747,#24748,#24749,#24750,#24751,#24752,#24753,
#24754,#24755,#24756,#24757,#24758,#24759,#24760,#24761,#24762,#24763)),
 .UNSPECIFIED.,.F.,.F.,.F.,(4,1,1,4),(4,1,1,1,1,1,1,1,1,1,1,1,1,1,1,4),
(0.,0.285714285714286,0.571428571428571,1.),(-4.47914967830435,-4.15921041556833,
-3.8392711528323,-3.51933189009628,-3.19939262736025,-2.98609978553623,
-2.77280694371222,-2.5595141018882,-2.13292841824016,-1.91963557641615,
-1.59969631368012,-1.2797570509441,-0.959817788208071,-0.639878525472046,
-0.319939262736021,4.7375248461733E-15),.UNSPECIFIED.);
#251=B_SPLINE_SURFACE_WITH_KNOTS('',3,3,((#25021,#25022,#25023,#25024,#25025,
#25026,#25027,#25028),(#25029,#25030,#25031,#25032,#25033,#25034,#25035,
#25036),(#25037,#25038,#25039,#25040,#25041,#25042,#25043,#25044),(#25045,
#25046,#25047,#25048,#25049,#25050,#25051,#25052),(#25053,#25054,#25055,
#25056,#25057,#25058,#25059,#25060),(#25061,#25062,#25063,#25064,#25065,
#25066,#25067,#25068)),.UNSPECIFIED.,.F.,.F.,.F.,(4,1,1,4),(4,1,1,1,1,4),
(0.,0.285714285714286,0.571428571428571,1.),(-1.49199371745016,-1.06570979817868,
-0.852567838542947,-0.426283919271474,-0.213141959635737,0.),
 .UNSPECIFIED.);
#252=B_SPLINE_SURFACE_WITH_KNOTS('',3,3,((#31387,#31388,#31389,#31390,#31391,
#31392,#31393,#31394,#31395,#31396,#31397,#31398,#31399,#31400,#31401,#31402,
#31403,#31404,#31405,#31406,#31407,#31408,#31409,#31410,#31411,#31412,#31413,
#31414,#31415,#31416,#31417,#31418,#31419,#31420,#31421,#31422,#31423,#31424,
#31425,#31426,#31427,#31428,#31429,#31430,#31431,#31432,#31433,#31434,#31435,
#31436,#31437,#31438,#31439,#31440,#31441,#31442,#31443,#31444,#31445,#31446,
#31447,#31448,#31449,#31450,#31451,#31452,#31453,#31454,#31455,#31456,#31457,
#31458,#31459,#31460,#31461,#31462,#31463,#31464,#31465,#31466,#31467,#31468,
#31469,#31470,#31471,#31472,#31473,#31474,#31475,#31476,#31477,#31478,#31479,
#31480,#31481,#31482,#31483,#31484,#31485,#31486,#31487,#31488,#31489,#31490,
#31491,#31492,#31493,#31494,#31495,#31496,#31497,#31498,#31499,#31500,#31501,
#31502,#31503,#31504,#31505,#31506,#31507,#31508,#31509,#31510,#31511,#31512,
#31513,#31514,#31515,#31516,#31517,#31518,#31519,#31520,#31521,#31522,#31523,
#31524,#31525,#31526,#31527,#31528,#31529,#31530,#31531,#31532,#31533,#31534,
#31535,#31536,#31537,#31538,#31539,#31540,#31541,#31542,#31543,#31544,#31545,
#31546,#31547,#31548,#31549,#31550,#31551,#31552,#31553,#31554,#31555,#31556,
#31557,#31558,#31559,#31560,#31561,#31562,#31563,#31564,#31565,#31566,#31567,
#31568,#31569,#31570,#31571,#31572,#31573,#31574,#31575,#31576,#31577,#31578,
#31579,#31580,#31581,#31582,#31583,#31584,#31585,#31586,#31587,#31588,#31589,
#31590,#31591,#31592,#31593,#31594,#31595,#31596,#31597,#31598,#31599,#31600,
#31601,#31602,#31603,#31604,#31605,#31606,#31607,#31608,#31609,#31610,#31611,
#31612,#31613,#31614,#31615,#31616,#31617,#31618,#31619,#31620,#31621,#31622,
#31623,#31624,#31625,#31626,#31627,#31628,#31629,#31630,#31631,#31632,#31633,
#31634,#31635,#31636,#31637,#31638,#31639,#31640,#31641,#31642,#31643,#31644,
#31645,#31646,#31647,#31648,#31649,#31650,#31651,#31652,#31653,#31654,#31655,
#31656,#31657,#31658,#31659,#31660,#31661,#31662,#31663,#31664,#31665,#31666,
#31667,#31668,#31669,#31670,#31671,#31672,#31673,#31674,#31675,#31676,#31677,
#31678,#31679,#31680,#31681,#31682,#31683,#31684,#31685,#31686,#31687,#31688,
#31689,#31690,#31691,#31692,#31693,#31694,#31695,#31696,#31697,#31698,#31699,
#31700,#31701,#31702,#31703,#31704,#31705,#31706,#31707,#31708,#31709,#31710,
#31711,#31712,#31713,#31714,#31715,#31716,#31717,#31718,#31719,#31720,#31721,
#31722,#31723,#31724,#31725,#31726,#31727,#31728,#31729,#31730,#31731,#31732,
#31733,#31734,#31735,#31736,#31737,#31738,#31739,#31740,#31741,#31742,#31743,
#31744,#31745,#31746,#31747,#31748,#31749,#31750,#31751,#31752,#31753,#31754,
#31755,#31756,#31757,#31758,#31759,#31760,#31761,#31762,#31763,#31764,#31765,
#31766,#31767,#31768,#31769,#31770,#31771,#31772,#31773,#31774,#31775,#31776,
#31777,#31778,#31779,#31780,#31781,#31782,#31783,#31784,#31785,#31786,#31787,
#31788,#31789,#31790,#31791,#31792,#31793,#31794,#31795,#31796,#31797,#31798,
#31799,#31800,#31801,#31802,#31803,#31804,#31805,#31806,#31807,#31808,#31809,
#31810,#31811,#31812,#31813,#31814,#31815,#31816,#31817,#31818,#31819,#31820,
#31821),(#31822,#31823,#31824,#31825,#31826,#31827,#31828,#31829,#31830,
#31831,#31832,#31833,#31834,#31835,#31836,#31837,#31838,#31839,#31840,#31841,
#31842,#31843,#31844,#31845,#31846,#31847,#31848,#31849,#31850,#31851,#31852,
#31853,#31854,#31855,#31856,#31857,#31858,#31859,#31860,#31861,#31862,#31863,
#31864,#31865,#31866,#31867,#31868,#31869,#31870,#31871,#31872,#31873,#31874,
#31875,#31876,#31877,#31878,#31879,#31880,#31881,#31882,#31883,#31884,#31885,
#31886,#31887,#31888,#31889,#31890,#31891,#31892,#31893,#31894,#31895,#31896,
#31897,#31898,#31899,#31900,#31901,#31902,#31903,#31904,#31905,#31906,#31907,
#31908,#31909,#31910,#31911,#31912,#31913,#31914,#31915,#31916,#31917,#31918,
#31919,#31920,#31921,#31922,#31923,#31924,#31925,#31926,#31927,#31928,#31929,
#31930,#31931,#31932,#31933,#31934,#31935,#31936,#31937,#31938,#31939,#31940,
#31941,#31942,#31943,#31944,#31945,#31946,#31947,#31948,#31949,#31950,#31951,
#31952,#31953,#31954,#31955,#31956,#31957,#31958,#31959,#31960,#31961,#31962,
#31963,#31964,#31965,#31966,#31967,#31968,#31969,#31970,#31971,#31972,#31973,
#31974,#31975,#31976,#31977,#31978,#31979,#31980,#31981,#31982,#31983,#31984,
#31985,#31986,#31987,#31988,#31989,#31990,#31991,#31992,#31993,#31994,#31995,
#31996,#31997,#31998,#31999,#32000,#32001,#32002,#32003,#32004,#32005,#32006,
#32007,#32008,#32009,#32010,#32011,#32012,#32013,#32014,#32015,#32016,#32017,
#32018,#32019,#32020,#32021,#32022,#32023,#32024,#32025,#32026,#32027,#32028,
#32029,#32030,#32031,#32032,#32033,#32034,#32035,#32036,#32037,#32038,#32039,
#32040,#32041,#32042,#32043,#32044,#32045,#32046,#32047,#32048,#32049,#32050,
#32051,#32052,#32053,#32054,#32055,#32056,#32057,#32058,#32059,#32060,#32061,
#32062,#32063,#32064,#32065,#32066,#32067,#32068,#32069,#32070,#32071,#32072,
#32073,#32074,#32075,#32076,#32077,#32078,#32079,#32080,#32081,#32082,#32083,
#32084,#32085,#32086,#32087,#32088,#32089,#32090,#32091,#32092,#32093,#32094,
#32095,#32096,#32097,#32098,#32099,#32100,#32101,#32102,#32103,#32104,#32105,
#32106,#32107,#32108,#32109,#32110,#32111,#32112,#32113,#32114,#32115,#32116,
#32117,#32118,#32119,#32120,#32121,#32122,#32123,#32124,#32125,#32126,#32127,
#32128,#32129,#32130,#32131,#32132,#32133,#32134,#32135,#32136,#32137,#32138,
#32139,#32140,#32141,#32142,#32143,#32144,#32145,#32146,#32147,#32148,#32149,
#32150,#32151,#32152,#32153,#32154,#32155,#32156,#32157,#32158,#32159,#32160,
#32161,#32162,#32163,#32164,#32165,#32166,#32167,#32168,#32169,#32170,#32171,
#32172,#32173,#32174,#32175,#32176,#32177,#32178,#32179,#32180,#32181,#32182,
#32183,#32184,#32185,#32186,#32187,#32188,#32189,#32190,#32191,#32192,#32193,
#32194,#32195,#32196,#32197,#32198,#32199,#32200,#32201,#32202,#32203,#32204,
#32205,#32206,#32207,#32208,#32209,#32210,#32211,#32212,#32213,#32214,#32215,
#32216,#32217,#32218,#32219,#32220,#32221,#32222,#32223,#32224,#32225,#32226,
#32227,#32228,#32229,#32230,#32231,#32232,#32233,#32234,#32235,#32236,#32237,
#32238,#32239,#32240,#32241,#32242,#32243,#32244,#32245,#32246,#32247,#32248,
#32249,#32250,#32251,#32252,#32253,#32254,#32255,#32256),(#32257,#32258,
#32259,#32260,#32261,#32262,#32263,#32264,#32265,#32266,#32267,#32268,#32269,
#32270,#32271,#32272,#32273,#32274,#32275,#32276,#32277,#32278,#32279,#32280,
#32281,#32282,#32283,#32284,#32285,#32286,#32287,#32288,#32289,#32290,#32291,
#32292,#32293,#32294,#32295,#32296,#32297,#32298,#32299,#32300,#32301,#32302,
#32303,#32304,#32305,#32306,#32307,#32308,#32309,#32310,#32311,#32312,#32313,
#32314,#32315,#32316,#32317,#32318,#32319,#32320,#32321,#32322,#32323,#32324,
#32325,#32326,#32327,#32328,#32329,#32330,#32331,#32332,#32333,#32334,#32335,
#32336,#32337,#32338,#32339,#32340,#32341,#32342,#32343,#32344,#32345,#32346,
#32347,#32348,#32349,#32350,#32351,#32352,#32353,#32354,#32355,#32356,#32357,
#32358,#32359,#32360,#32361,#32362,#32363,#32364,#32365,#32366,#32367,#32368,
#32369,#32370,#32371,#32372,#32373,#32374,#32375,#32376,#32377,#32378,#32379,
#32380,#32381,#32382,#32383,#32384,#32385,#32386,#32387,#32388,#32389,#32390,
#32391,#32392,#32393,#32394,#32395,#32396,#32397,#32398,#32399,#32400,#32401,
#32402,#32403,#32404,#32405,#32406,#32407,#32408,#32409,#32410,#32411,#32412,
#32413,#32414,#32415,#32416,#32417,#32418,#32419,#32420,#32421,#32422,#32423,
#32424,#32425,#32426,#32427,#32428,#32429,#32430,#32431,#32432,#32433,#32434,
#32435,#32436,#32437,#32438,#32439,#32440,#32441,#32442,#32443,#32444,#32445,
#32446,#32447,#32448,#32449,#32450,#32451,#32452,#32453,#32454,#32455,#32456,
#32457,#32458,#32459,#32460,#32461,#32462,#32463,#32464,#32465,#32466,#32467,
#32468,#32469,#32470,#32471,#32472,#32473,#32474,#32475,#32476,#32477,#32478,
#32479,#32480,#32481,#32482,#32483,#32484,#32485,#32486,#32487,#32488,#32489,
#32490,#32491,#32492,#32493,#32494,#32495,#32496,#32497,#32498,#32499,#32500,
#32501,#32502,#32503,#32504,#32505,#32506,#32507,#32508,#32509,#32510,#32511,
#32512,#32513,#32514,#32515,#32516,#32517,#32518,#32519,#32520,#32521,#32522,
#32523,#32524,#32525,#32526,#32527,#32528,#32529,#32530,#32531,#32532,#32533,
#32534,#32535,#32536,#32537,#32538,#32539,#32540,#32541,#32542,#32543,#32544,
#32545,#32546,#32547,#32548,#32549,#32550,#32551,#32552,#32553,#32554,#32555,
#32556,#32557,#32558,#32559,#32560,#32561,#32562,#32563,#32564,#32565,#32566,
#32567,#32568,#32569,#32570,#32571,#32572,#32573,#32574,#32575,#32576,#32577,
#32578,#32579,#32580,#32581,#32582,#32583,#32584,#32585,#32586,#32587,#32588,
#32589,#32590,#32591,#32592,#32593,#32594,#32595,#32596,#32597,#32598,#32599,
#32600,#32601,#32602,#32603,#32604,#32605,#32606,#32607,#32608,#32609,#32610,
#32611,#32612,#32613,#32614,#32615,#32616,#32617,#32618,#32619,#32620,#32621,
#32622,#32623,#32624,#32625,#32626,#32627,#32628,#32629,#32630,#32631,#32632,
#32633,#32634,#32635,#32636,#32637,#32638,#32639,#32640,#32641,#32642,#32643,
#32644,#32645,#32646,#32647,#32648,#32649,#32650,#32651,#32652,#32653,#32654,
#32655,#32656,#32657,#32658,#32659,#32660,#32661,#32662,#32663,#32664,#32665,
#32666,#32667,#32668,#32669,#32670,#32671,#32672,#32673,#32674,#32675,#32676,
#32677,#32678,#32679,#32680,#32681,#32682,#32683,#32684,#32685,#32686,#32687,
#32688,#32689,#32690,#32691),(#32692,#32693,#32694,#32695,#32696,#32697,
#32698,#32699,#32700,#32701,#32702,#32703,#32704,#32705,#32706,#32707,#32708,
#32709,#32710,#32711,#32712,#32713,#32714,#32715,#32716,#32717,#32718,#32719,
#32720,#32721,#32722,#32723,#32724,#32725,#32726,#32727,#32728,#32729,#32730,
#32731,#32732,#32733,#32734,#32735,#32736,#32737,#32738,#32739,#32740,#32741,
#32742,#32743,#32744,#32745,#32746,#32747,#32748,#32749,#32750,#32751,#32752,
#32753,#32754,#32755,#32756,#32757,#32758,#32759,#32760,#32761,#32762,#32763,
#32764,#32765,#32766,#32767,#32768,#32769,#32770,#32771,#32772,#32773,#32774,
#32775,#32776,#32777,#32778,#32779,#32780,#32781,#32782,#32783,#32784,#32785,
#32786,#32787,#32788,#32789,#32790,#32791,#32792,#32793,#32794,#32795,#32796,
#32797,#32798,#32799,#32800,#32801,#32802,#32803,#32804,#32805,#32806,#32807,
#32808,#32809,#32810,#32811,#32812,#32813,#32814,#32815,#32816,#32817,#32818,
#32819,#32820,#32821,#32822,#32823,#32824,#32825,#32826,#32827,#32828,#32829,
#32830,#32831,#32832,#32833,#32834,#32835,#32836,#32837,#32838,#32839,#32840,
#32841,#32842,#32843,#32844,#32845,#32846,#32847,#32848,#32849,#32850,#32851,
#32852,#32853,#32854,#32855,#32856,#32857,#32858,#32859,#32860,#32861,#32862,
#32863,#32864,#32865,#32866,#32867,#32868,#32869,#32870,#32871,#32872,#32873,
#32874,#32875,#32876,#32877,#32878,#32879,#32880,#32881,#32882,#32883,#32884,
#32885,#32886,#32887,#32888,#32889,#32890,#32891,#32892,#32893,#32894,#32895,
#32896,#32897,#32898,#32899,#32900,#32901,#32902,#32903,#32904,#32905,#32906,
#32907,#32908,#32909,#32910,#32911,#32912,#32913,#32914,#32915,#32916,#32917,
#32918,#32919,#32920,#32921,#32922,#32923,#32924,#32925,#32926,#32927,#32928,
#32929,#32930,#32931,#32932,#32933,#32934,#32935,#32936,#32937,#32938,#32939,
#32940,#32941,#32942,#32943,#32944,#32945,#32946,#32947,#32948,#32949,#32950,
#32951,#32952,#32953,#32954,#32955,#32956,#32957,#32958,#32959,#32960,#32961,
#32962,#32963,#32964,#32965,#32966,#32967,#32968,#32969,#32970,#32971,#32972,
#32973,#32974,#32975,#32976,#32977,#32978,#32979,#32980,#32981,#32982,#32983,
#32984,#32985,#32986,#32987,#32988,#32989,#32990,#32991,#32992,#32993,#32994,
#32995,#32996,#32997,#32998,#32999,#33000,#33001,#33002,#33003,#33004,#33005,
#33006,#33007,#33008,#33009,#33010,#33011,#33012,#33013,#33014,#33015,#33016,
#33017,#33018,#33019,#33020,#33021,#33022,#33023,#33024,#33025,#33026,#33027,
#33028,#33029,#33030,#33031,#33032,#33033,#33034,#33035,#33036,#33037,#33038,
#33039,#33040,#33041,#33042,#33043,#33044,#33045,#33046,#33047,#33048,#33049,
#33050,#33051,#33052,#33053,#33054,#33055,#33056,#33057,#33058,#33059,#33060,
#33061,#33062,#33063,#33064,#33065,#33066,#33067,#33068,#33069,#33070,#33071,
#33072,#33073,#33074,#33075,#33076,#33077,#33078,#33079,#33080,#33081,#33082,
#33083,#33084,#33085,#33086,#33087,#33088,#33089,#33090,#33091,#33092,#33093,
#33094,#33095,#33096,#33097,#33098,#33099,#33100,#33101,#33102,#33103,#33104,
#33105,#33106,#33107,#33108,#33109,#33110,#33111,#33112,#33113,#33114,#33115,
#33116,#33117,#33118,#33119,#33120,#33121,#33122,#33123,#33124,#33125,#33126)),
 .UNSPECIFIED.,.F.,.F.,.F.,(4,4),(4,1,1,1,1,1,1,1,1,1,1,1,1,1,1,1,1,1,1,
1,1,1,1,1,1,1,1,1,1,1,1,1,1,1,1,1,1,1,1,1,1,1,1,1,1,1,1,1,1,1,1,1,1,1,1,
1,1,1,1,1,1,1,1,1,1,1,1,1,1,1,1,1,1,1,1,1,1,1,1,1,1,1,1,1,1,1,1,1,1,1,1,
1,1,1,1,1,1,1,1,1,1,1,1,1,1,1,1,1,1,1,1,1,1,1,1,1,1,1,1,1,1,1,1,1,1,1,1,
1,1,1,1,1,1,1,1,1,1,1,1,1,1,1,1,1,1,1,1,1,1,1,1,1,1,1,1,1,1,1,1,1,1,1,1,
1,1,1,1,1,1,1,1,1,1,1,1,1,1,1,1,1,1,1,1,1,1,1,1,1,1,1,1,1,1,1,1,1,1,1,1,
1,1,1,1,1,1,1,1,1,1,1,1,1,1,1,1,1,1,1,1,1,1,1,1,1,1,1,1,1,1,1,1,1,1,1,1,
1,1,1,1,1,1,1,1,1,1,1,1,1,1,1,1,1,1,1,1,1,1,1,1,1,1,1,1,1,1,1,1,1,1,1,1,
1,1,1,1,1,1,1,1,1,1,1,1,1,1,1,1,1,1,1,1,1,1,1,1,1,1,1,1,1,1,1,1,1,1,1,1,
1,1,1,1,1,1,1,1,1,1,1,1,1,1,1,1,1,1,1,1,1,1,1,1,1,1,1,1,1,1,1,1,1,1,1,1,
1,1,1,1,1,1,1,1,1,1,1,1,1,1,1,1,1,1,1,1,1,1,1,1,1,1,1,1,1,1,1,1,1,1,1,1,
1,1,1,1,1,1,1,1,1,1,1,1,1,1,1,1,1,1,1,1,1,1,1,1,1,1,1,1,1,1,1,1,1,1,1,1,
1,1,1,1,1,1,1,1,1,1,1,1,1,1,1,1,1,4),(0.,0.115296848757168),(8.30592286723195,
8.80591593374569,9.30590900025942,9.80590206677316,10.3058951332869,10.8058881998006,
11.3058812663144,11.8058743328281,12.3058673993418,12.8058604658556,13.3058535323693,
13.805846598883,14.3058396653968,14.8058327319105,15.3058257984242,15.805818864938,
16.3058119314517,16.8058049979655,17.3057980644792,17.8057911309929,18.3057841975067,
18.8057772640204,19.3057703305341,19.8057633970479,20.3057564635616,20.8057495300753,
21.3057425965891,21.8057356631028,22.3057287296165,22.8057217961303,23.305714862644,
23.8057079291577,24.3057009956715,24.8056940621852,25.305687128699,25.8056801952127,
26.3056732617264,26.8056663282402,27.3056593947539,27.8056524612676,28.3056455277814,
28.8056385942951,29.3056316608088,29.8056247273226,30.3056177938363,30.80561086035,
31.3056039268638,31.8055969933775,32.3055900598912,32.805583126405,33.3055761929187,
33.8055692594324,34.3055623259462,34.8055553924599,35.3055484589737,35.8055415254874,
36.3055345920011,36.8055276585149,37.3055207250286,37.8055137915423,38.3055068580561,
38.8054999245698,39.3054929910835,39.8054860575973,40.305479124111,40.8054721906247,
41.3054652571385,41.8054583236522,42.305451390166,42.8054444566797,43.3054375231934,
43.8054305897072,44.3054236562209,44.8054167227346,45.3054097892484,45.8054028557621,
46.3053959222758,46.8053889887896,47.3053820553033,47.805375121817,48.3053681883308,
48.8053612548445,49.3053543213582,49.805347387872,50.3053404543857,50.8053335208995,
51.3053265874132,51.8053196539269,52.3053127204407,52.8053057869544,53.3052988534681,
53.8052919199819,54.3052849864956,54.8052780530093,55.3052711195231,55.8052641860368,
56.3052572525505,56.8052503190643,57.305243385578,57.8052364520917,58.3052295186055,
58.8052225851192,59.3052156516329,59.8052087181467,60.3052017846604,60.8051948511742,
61.3051879176879,61.8051809842016,62.3051740507154,62.8051671172291,63.3051601837428,
63.8051532502566,64.3051463167703,64.805139383284,65.3051324497978,65.8051255163115,
66.3051185828252,66.805111649339,67.3051047158527,67.8050977823664,68.3050908488802,
68.8050839153939,69.3050769819077,69.8050700484214,70.3050631149351,70.8050561814489,
71.3050492479626,71.8050423144763,72.3050353809901,72.8050284475038,73.3050215140175,
73.8050145805313,74.305007647045,74.8050007135587,75.3049937800725,75.8049868465862,
76.3049799131,76.8049729796137,77.3049660461274,77.8049591126412,78.3049521791549,
78.8049452456686,79.3049383121824,79.8049313786961,80.3049244452098,80.8049175117236,
81.3049105782373,81.804903644751,82.3048967112648,82.8048897777785,83.3048828442923,
83.804875910806,84.3048689773197,84.8048620438335,85.3048551103472,85.8048481768609,
86.3048412433747,86.8048343098884,87.3048273764021,87.8048204429159,88.3048135094296,
88.8048065759433,89.3047996424571,89.8047927089708,90.3047857754845,90.8047788419983,
91.304771908512,91.8047649750257,92.3047580415395,92.8047511080532,93.3047441745669,
93.8047372410807,94.3047303075944,94.8047233741082,95.3047164406219,95.8047095071356,
96.3047025736494,96.8046956401631,97.3046887066768,97.8046817731906,98.3046748397043,
98.804667906218,99.3046609727318,99.8046540392455,100.304647105759,100.804640172273,
101.304633238787,101.8046263053,102.304619371814,102.804612438328,103.304605504842,
103.804598571355,104.304591637869,104.804584704383,105.304577770897,105.80457083741,
106.304563903924,106.804556970438,107.304550036952,107.804543103465,108.304536169979,
108.804529236493,109.304522303006,109.80451536952,110.304508436034,110.804501502548,
111.304494569061,111.804487635575,112.304480702089,112.804473768603,113.304466835116,
113.80445990163,114.304452968144,114.804446034658,115.304439101171,115.804432167685,
116.304425234199,116.804418300713,117.304411367226,117.80440443374,118.304397500254,
118.804390566767,119.304383633281,119.804376699795,120.304369766309,120.804362832822,
121.304355899336,121.80434896585,122.304342032364,122.804335098877,123.304328165391,
123.804321231905,124.304314298419,124.804307364932,125.304300431446,125.80429349796,
126.304286564473,126.804279630987,127.304272697501,127.804265764015,128.304258830528,
128.804251897042,129.304244963556,129.80423803007,130.304231096583,130.804224163097,
131.304217229611,131.804210296125,132.304203362638,132.804196429152,133.304189495666,
133.80418256218,134.304175628693,134.804168695207,135.304161761721,135.804154828234,
136.304147894748,136.804140961262,137.304134027776,137.804127094289,138.304120160803,
138.804113227317,139.304106293831,139.804099360344,140.304092426858,140.804085493372,
141.304078559886,141.804071626399,142.304064692913,142.804057759427,143.30405082594,
143.804043892454,144.304036958968,144.804030025482,145.304023091995,145.804016158509,
146.304009225023,146.804002291537,147.30399535805,147.803988424564,148.303981491078,
148.803974557592,149.303967624105,149.803960690619,150.303953757133,150.803946823646,
151.30393989016,151.803932956674,152.303926023188,152.803919089701,153.303912156215,
153.803905222729,154.303898289243,154.803891355756,155.30388442227,155.803877488784,
156.303870555298,156.803863621811,157.303856688325,157.803849754839,158.303842821353,
158.803835887866,159.30382895438,159.803822020894,160.303815087407,160.803808153921,
161.303801220435,161.803794286949,162.303787353462,162.803780419976,163.30377348649,
163.803766553004,164.303759619517,164.803752686031,165.303745752545,165.803738819059,
166.303731885572,166.803724952086,167.3037180186,167.803711085113,168.303704151627,
168.803697218141,169.303690284655,169.803683351168,170.303676417682,170.803669484196,
171.30366255071,171.803655617223,172.303648683737,172.803641750251,173.303634816765,
173.803627883278,174.303620949792,174.803614016306,175.30360708282,175.803600149333,
176.303593215847,176.803586282361,177.303579348874,177.803572415388,178.303565481902,
178.803558548416,179.303551614929,179.803544681443,180.303537747957,180.803530814471,
181.303523880984,181.803516947498,182.303510014012,182.803503080526,183.303496147039,
183.803489213553,184.303482280067,184.803475346581,185.303468413094,185.803461479608,
186.303454546122,186.803447612635,187.303440679149,187.803433745663,188.303426812177,
188.80341987869,189.303412945204,189.803406011718,190.303399078232,190.803392144745,
191.303385211259,191.803378277773,192.303371344287,192.8033644108,193.303357477314,
193.803350543828,194.303343610341,194.803336676855,195.303329743369,195.803322809883,
196.303315876396,196.80330894291,197.303302009424,197.803295075938,198.303288142451,
198.803281208965,199.303274275479,199.803267341993,200.303260408506,200.80325347502,
201.303246541534,201.803239608047,202.303232674561,202.803225741075,203.303218807589,
203.803211874102,204.303204940616,204.80319800713,205.303191073644,205.803184140157,
206.303177206671,206.803170273185,207.303163339699,207.803156406212,208.303149472726,
208.80314253924,209.303135605754,209.803128672267,210.303121738781,210.803114805295,
211.303107871808,211.803100938322,212.303094004836,212.80308707135,213.303080137863,
213.803073204377,214.303066270891,214.803059337405,215.303052403918,215.803045470432,
216.303038536946,216.80303160346,217.303024669973,217.803017736487,218.303010803001,
218.803003869514,219.302996936028,219.802990002542,220.302983069056,220.802976135569,
221.302969202083,221.802962268597,222.302955335111,222.802948401624,223.302941468138,
223.802934534652,224.302927601166),.UNSPECIFIED.);
#253=B_SPLINE_SURFACE_WITH_KNOTS('',3,3,((#33529,#33530,#33531,#33532,#33533,
#33534,#33535,#33536,#33537,#33538,#33539,#33540,#33541,#33542,#33543,#33544,
#33545,#33546,#33547,#33548,#33549,#33550,#33551,#33552,#33553,#33554,#33555,
#33556,#33557,#33558,#33559,#33560,#33561,#33562,#33563,#33564,#33565,#33566,
#33567,#33568,#33569,#33570,#33571,#33572,#33573,#33574,#33575,#33576,#33577,
#33578,#33579,#33580,#33581,#33582,#33583,#33584,#33585,#33586,#33587,#33588,
#33589,#33590,#33591,#33592,#33593,#33594,#33595,#33596,#33597,#33598,#33599,
#33600,#33601,#33602,#33603,#33604,#33605,#33606,#33607,#33608,#33609,#33610,
#33611,#33612,#33613,#33614,#33615,#33616,#33617,#33618,#33619,#33620,#33621,
#33622,#33623,#33624,#33625,#33626,#33627,#33628,#33629,#33630,#33631,#33632,
#33633,#33634,#33635,#33636,#33637,#33638,#33639,#33640,#33641,#33642,#33643,
#33644,#33645,#33646,#33647,#33648,#33649,#33650,#33651,#33652,#33653,#33654,
#33655,#33656,#33657,#33658,#33659,#33660,#33661,#33662,#33663,#33664,#33665,
#33666,#33667,#33668,#33669,#33670,#33671,#33672,#33673,#33674,#33675,#33676,
#33677,#33678,#33679,#33680,#33681,#33682,#33683,#33684,#33685,#33686,#33687,
#33688,#33689,#33690,#33691,#33692,#33693,#33694,#33695,#33696,#33697,#33698,
#33699,#33700,#33701,#33702,#33703,#33704,#33705,#33706,#33707,#33708,#33709,
#33710,#33711,#33712,#33713,#33714,#33715,#33716,#33717,#33718,#33719,#33720,
#33721,#33722,#33723,#33724,#33725,#33726,#33727,#33728,#33729,#33730,#33731,
#33732,#33733,#33734,#33735,#33736,#33737,#33738,#33739,#33740,#33741,#33742,
#33743,#33744,#33745,#33746,#33747,#33748,#33749,#33750,#33751,#33752,#33753,
#33754,#33755,#33756,#33757,#33758,#33759,#33760,#33761,#33762,#33763,#33764,
#33765,#33766,#33767,#33768,#33769,#33770,#33771,#33772,#33773,#33774,#33775,
#33776,#33777,#33778,#33779,#33780,#33781,#33782,#33783,#33784,#33785,#33786,
#33787,#33788,#33789,#33790,#33791,#33792,#33793,#33794,#33795,#33796,#33797,
#33798,#33799,#33800,#33801,#33802,#33803,#33804,#33805,#33806,#33807,#33808,
#33809,#33810,#33811,#33812,#33813,#33814,#33815,#33816,#33817,#33818,#33819,
#33820,#33821,#33822,#33823,#33824,#33825,#33826,#33827,#33828,#33829,#33830,
#33831,#33832,#33833,#33834,#33835,#33836,#33837,#33838,#33839,#33840,#33841,
#33842,#33843,#33844,#33845,#33846,#33847,#33848,#33849,#33850,#33851,#33852,
#33853,#33854,#33855,#33856,#33857,#33858,#33859,#33860,#33861,#33862,#33863,
#33864,#33865,#33866,#33867,#33868,#33869,#33870,#33871,#33872,#33873,#33874,
#33875,#33876,#33877,#33878,#33879,#33880,#33881,#33882,#33883,#33884,#33885,
#33886,#33887,#33888,#33889,#33890,#33891,#33892,#33893,#33894,#33895,#33896,
#33897,#33898,#33899,#33900,#33901,#33902,#33903,#33904,#33905,#33906,#33907,
#33908,#33909,#33910,#33911,#33912,#33913,#33914,#33915,#33916,#33917,#33918,
#33919,#33920,#33921,#33922,#33923,#33924,#33925,#33926,#33927,#33928,#33929,
#33930,#33931,#33932,#33933,#33934,#33935,#33936,#33937,#33938,#33939,#33940,
#33941,#33942,#33943,#33944,#33945,#33946,#33947,#33948,#33949,#33950,#33951,
#33952,#33953,#33954,#33955,#33956,#33957,#33958,#33959,#33960,#33961,#33962,
#33963),(#33964,#33965,#33966,#33967,#33968,#33969,#33970,#33971,#33972,
#33973,#33974,#33975,#33976,#33977,#33978,#33979,#33980,#33981,#33982,#33983,
#33984,#33985,#33986,#33987,#33988,#33989,#33990,#33991,#33992,#33993,#33994,
#33995,#33996,#33997,#33998,#33999,#34000,#34001,#34002,#34003,#34004,#34005,
#34006,#34007,#34008,#34009,#34010,#34011,#34012,#34013,#34014,#34015,#34016,
#34017,#34018,#34019,#34020,#34021,#34022,#34023,#34024,#34025,#34026,#34027,
#34028,#34029,#34030,#34031,#34032,#34033,#34034,#34035,#34036,#34037,#34038,
#34039,#34040,#34041,#34042,#34043,#34044,#34045,#34046,#34047,#34048,#34049,
#34050,#34051,#34052,#34053,#34054,#34055,#34056,#34057,#34058,#34059,#34060,
#34061,#34062,#34063,#34064,#34065,#34066,#34067,#34068,#34069,#34070,#34071,
#34072,#34073,#34074,#34075,#34076,#34077,#34078,#34079,#34080,#34081,#34082,
#34083,#34084,#34085,#34086,#34087,#34088,#34089,#34090,#34091,#34092,#34093,
#34094,#34095,#34096,#34097,#34098,#34099,#34100,#34101,#34102,#34103,#34104,
#34105,#34106,#34107,#34108,#34109,#34110,#34111,#34112,#34113,#34114,#34115,
#34116,#34117,#34118,#34119,#34120,#34121,#34122,#34123,#34124,#34125,#34126,
#34127,#34128,#34129,#34130,#34131,#34132,#34133,#34134,#34135,#34136,#34137,
#34138,#34139,#34140,#34141,#34142,#34143,#34144,#34145,#34146,#34147,#34148,
#34149,#34150,#34151,#34152,#34153,#34154,#34155,#34156,#34157,#34158,#34159,
#34160,#34161,#34162,#34163,#34164,#34165,#34166,#34167,#34168,#34169,#34170,
#34171,#34172,#34173,#34174,#34175,#34176,#34177,#34178,#34179,#34180,#34181,
#34182,#34183,#34184,#34185,#34186,#34187,#34188,#34189,#34190,#34191,#34192,
#34193,#34194,#34195,#34196,#34197,#34198,#34199,#34200,#34201,#34202,#34203,
#34204,#34205,#34206,#34207,#34208,#34209,#34210,#34211,#34212,#34213,#34214,
#34215,#34216,#34217,#34218,#34219,#34220,#34221,#34222,#34223,#34224,#34225,
#34226,#34227,#34228,#34229,#34230,#34231,#34232,#34233,#34234,#34235,#34236,
#34237,#34238,#34239,#34240,#34241,#34242,#34243,#34244,#34245,#34246,#34247,
#34248,#34249,#34250,#34251,#34252,#34253,#34254,#34255,#34256,#34257,#34258,
#34259,#34260,#34261,#34262,#34263,#34264,#34265,#34266,#34267,#34268,#34269,
#34270,#34271,#34272,#34273,#34274,#34275,#34276,#34277,#34278,#34279,#34280,
#34281,#34282,#34283,#34284,#34285,#34286,#34287,#34288,#34289,#34290,#34291,
#34292,#34293,#34294,#34295,#34296,#34297,#34298,#34299,#34300,#34301,#34302,
#34303,#34304,#34305,#34306,#34307,#34308,#34309,#34310,#34311,#34312,#34313,
#34314,#34315,#34316,#34317,#34318,#34319,#34320,#34321,#34322,#34323,#34324,
#34325,#34326,#34327,#34328,#34329,#34330,#34331,#34332,#34333,#34334,#34335,
#34336,#34337,#34338,#34339,#34340,#34341,#34342,#34343,#34344,#34345,#34346,
#34347,#34348,#34349,#34350,#34351,#34352,#34353,#34354,#34355,#34356,#34357,
#34358,#34359,#34360,#34361,#34362,#34363,#34364,#34365,#34366,#34367,#34368,
#34369,#34370,#34371,#34372,#34373,#34374,#34375,#34376,#34377,#34378,#34379,
#34380,#34381,#34382,#34383,#34384,#34385,#34386,#34387,#34388,#34389,#34390,
#34391,#34392,#34393,#34394,#34395,#34396,#34397,#34398),(#34399,#34400,
#34401,#34402,#34403,#34404,#34405,#34406,#34407,#34408,#34409,#34410,#34411,
#34412,#34413,#34414,#34415,#34416,#34417,#34418,#34419,#34420,#34421,#34422,
#34423,#34424,#34425,#34426,#34427,#34428,#34429,#34430,#34431,#34432,#34433,
#34434,#34435,#34436,#34437,#34438,#34439,#34440,#34441,#34442,#34443,#34444,
#34445,#34446,#34447,#34448,#34449,#34450,#34451,#34452,#34453,#34454,#34455,
#34456,#34457,#34458,#34459,#34460,#34461,#34462,#34463,#34464,#34465,#34466,
#34467,#34468,#34469,#34470,#34471,#34472,#34473,#34474,#34475,#34476,#34477,
#34478,#34479,#34480,#34481,#34482,#34483,#34484,#34485,#34486,#34487,#34488,
#34489,#34490,#34491,#34492,#34493,#34494,#34495,#34496,#34497,#34498,#34499,
#34500,#34501,#34502,#34503,#34504,#34505,#34506,#34507,#34508,#34509,#34510,
#34511,#34512,#34513,#34514,#34515,#34516,#34517,#34518,#34519,#34520,#34521,
#34522,#34523,#34524,#34525,#34526,#34527,#34528,#34529,#34530,#34531,#34532,
#34533,#34534,#34535,#34536,#34537,#34538,#34539,#34540,#34541,#34542,#34543,
#34544,#34545,#34546,#34547,#34548,#34549,#34550,#34551,#34552,#34553,#34554,
#34555,#34556,#34557,#34558,#34559,#34560,#34561,#34562,#34563,#34564,#34565,
#34566,#34567,#34568,#34569,#34570,#34571,#34572,#34573,#34574,#34575,#34576,
#34577,#34578,#34579,#34580,#34581,#34582,#34583,#34584,#34585,#34586,#34587,
#34588,#34589,#34590,#34591,#34592,#34593,#34594,#34595,#34596,#34597,#34598,
#34599,#34600,#34601,#34602,#34603,#34604,#34605,#34606,#34607,#34608,#34609,
#34610,#34611,#34612,#34613,#34614,#34615,#34616,#34617,#34618,#34619,#34620,
#34621,#34622,#34623,#34624,#34625,#34626,#34627,#34628,#34629,#34630,#34631,
#34632,#34633,#34634,#34635,#34636,#34637,#34638,#34639,#34640,#34641,#34642,
#34643,#34644,#34645,#34646,#34647,#34648,#34649,#34650,#34651,#34652,#34653,
#34654,#34655,#34656,#34657,#34658,#34659,#34660,#34661,#34662,#34663,#34664,
#34665,#34666,#34667,#34668,#34669,#34670,#34671,#34672,#34673,#34674,#34675,
#34676,#34677,#34678,#34679,#34680,#34681,#34682,#34683,#34684,#34685,#34686,
#34687,#34688,#34689,#34690,#34691,#34692,#34693,#34694,#34695,#34696,#34697,
#34698,#34699,#34700,#34701,#34702,#34703,#34704,#34705,#34706,#34707,#34708,
#34709,#34710,#34711,#34712,#34713,#34714,#34715,#34716,#34717,#34718,#34719,
#34720,#34721,#34722,#34723,#34724,#34725,#34726,#34727,#34728,#34729,#34730,
#34731,#34732,#34733,#34734,#34735,#34736,#34737,#34738,#34739,#34740,#34741,
#34742,#34743,#34744,#34745,#34746,#34747,#34748,#34749,#34750,#34751,#34752,
#34753,#34754,#34755,#34756,#34757,#34758,#34759,#34760,#34761,#34762,#34763,
#34764,#34765,#34766,#34767,#34768,#34769,#34770,#34771,#34772,#34773,#34774,
#34775,#34776,#34777,#34778,#34779,#34780,#34781,#34782,#34783,#34784,#34785,
#34786,#34787,#34788,#34789,#34790,#34791,#34792,#34793,#34794,#34795,#34796,
#34797,#34798,#34799,#34800,#34801,#34802,#34803,#34804,#34805,#34806,#34807,
#34808,#34809,#34810,#34811,#34812,#34813,#34814,#34815,#34816,#34817,#34818,
#34819,#34820,#34821,#34822,#34823,#34824,#34825,#34826,#34827,#34828,#34829,
#34830,#34831,#34832,#34833),(#34834,#34835,#34836,#34837,#34838,#34839,
#34840,#34841,#34842,#34843,#34844,#34845,#34846,#34847,#34848,#34849,#34850,
#34851,#34852,#34853,#34854,#34855,#34856,#34857,#34858,#34859,#34860,#34861,
#34862,#34863,#34864,#34865,#34866,#34867,#34868,#34869,#34870,#34871,#34872,
#34873,#34874,#34875,#34876,#34877,#34878,#34879,#34880,#34881,#34882,#34883,
#34884,#34885,#34886,#34887,#34888,#34889,#34890,#34891,#34892,#34893,#34894,
#34895,#34896,#34897,#34898,#34899,#34900,#34901,#34902,#34903,#34904,#34905,
#34906,#34907,#34908,#34909,#34910,#34911,#34912,#34913,#34914,#34915,#34916,
#34917,#34918,#34919,#34920,#34921,#34922,#34923,#34924,#34925,#34926,#34927,
#34928,#34929,#34930,#34931,#34932,#34933,#34934,#34935,#34936,#34937,#34938,
#34939,#34940,#34941,#34942,#34943,#34944,#34945,#34946,#34947,#34948,#34949,
#34950,#34951,#34952,#34953,#34954,#34955,#34956,#34957,#34958,#34959,#34960,
#34961,#34962,#34963,#34964,#34965,#34966,#34967,#34968,#34969,#34970,#34971,
#34972,#34973,#34974,#34975,#34976,#34977,#34978,#34979,#34980,#34981,#34982,
#34983,#34984,#34985,#34986,#34987,#34988,#34989,#34990,#34991,#34992,#34993,
#34994,#34995,#34996,#34997,#34998,#34999,#35000,#35001,#35002,#35003,#35004,
#35005,#35006,#35007,#35008,#35009,#35010,#35011,#35012,#35013,#35014,#35015,
#35016,#35017,#35018,#35019,#35020,#35021,#35022,#35023,#35024,#35025,#35026,
#35027,#35028,#35029,#35030,#35031,#35032,#35033,#35034,#35035,#35036,#35037,
#35038,#35039,#35040,#35041,#35042,#35043,#35044,#35045,#35046,#35047,#35048,
#35049,#35050,#35051,#35052,#35053,#35054,#35055,#35056,#35057,#35058,#35059,
#35060,#35061,#35062,#35063,#35064,#35065,#35066,#35067,#35068,#35069,#35070,
#35071,#35072,#35073,#35074,#35075,#35076,#35077,#35078,#35079,#35080,#35081,
#35082,#35083,#35084,#35085,#35086,#35087,#35088,#35089,#35090,#35091,#35092,
#35093,#35094,#35095,#35096,#35097,#35098,#35099,#35100,#35101,#35102,#35103,
#35104,#35105,#35106,#35107,#35108,#35109,#35110,#35111,#35112,#35113,#35114,
#35115,#35116,#35117,#35118,#35119,#35120,#35121,#35122,#35123,#35124,#35125,
#35126,#35127,#35128,#35129,#35130,#35131,#35132,#35133,#35134,#35135,#35136,
#35137,#35138,#35139,#35140,#35141,#35142,#35143,#35144,#35145,#35146,#35147,
#35148,#35149,#35150,#35151,#35152,#35153,#35154,#35155,#35156,#35157,#35158,
#35159,#35160,#35161,#35162,#35163,#35164,#35165,#35166,#35167,#35168,#35169,
#35170,#35171,#35172,#35173,#35174,#35175,#35176,#35177,#35178,#35179,#35180,
#35181,#35182,#35183,#35184,#35185,#35186,#35187,#35188,#35189,#35190,#35191,
#35192,#35193,#35194,#35195,#35196,#35197,#35198,#35199,#35200,#35201,#35202,
#35203,#35204,#35205,#35206,#35207,#35208,#35209,#35210,#35211,#35212,#35213,
#35214,#35215,#35216,#35217,#35218,#35219,#35220,#35221,#35222,#35223,#35224,
#35225,#35226,#35227,#35228,#35229,#35230,#35231,#35232,#35233,#35234,#35235,
#35236,#35237,#35238,#35239,#35240,#35241,#35242,#35243,#35244,#35245,#35246,
#35247,#35248,#35249,#35250,#35251,#35252,#35253,#35254,#35255,#35256,#35257,
#35258,#35259,#35260,#35261,#35262,#35263,#35264,#35265,#35266,#35267,#35268)),
 .UNSPECIFIED.,.F.,.F.,.F.,(4,4),(4,1,1,1,1,1,1,1,1,1,1,1,1,1,1,1,1,1,1,
1,1,1,1,1,1,1,1,1,1,1,1,1,1,1,1,1,1,1,1,1,1,1,1,1,1,1,1,1,1,1,1,1,1,1,1,
1,1,1,1,1,1,1,1,1,1,1,1,1,1,1,1,1,1,1,1,1,1,1,1,1,1,1,1,1,1,1,1,1,1,1,1,
1,1,1,1,1,1,1,1,1,1,1,1,1,1,1,1,1,1,1,1,1,1,1,1,1,1,1,1,1,1,1,1,1,1,1,1,
1,1,1,1,1,1,1,1,1,1,1,1,1,1,1,1,1,1,1,1,1,1,1,1,1,1,1,1,1,1,1,1,1,1,1,1,
1,1,1,1,1,1,1,1,1,1,1,1,1,1,1,1,1,1,1,1,1,1,1,1,1,1,1,1,1,1,1,1,1,1,1,1,
1,1,1,1,1,1,1,1,1,1,1,1,1,1,1,1,1,1,1,1,1,1,1,1,1,1,1,1,1,1,1,1,1,1,1,1,
1,1,1,1,1,1,1,1,1,1,1,1,1,1,1,1,1,1,1,1,1,1,1,1,1,1,1,1,1,1,1,1,1,1,1,1,
1,1,1,1,1,1,1,1,1,1,1,1,1,1,1,1,1,1,1,1,1,1,1,1,1,1,1,1,1,1,1,1,1,1,1,1,
1,1,1,1,1,1,1,1,1,1,1,1,1,1,1,1,1,1,1,1,1,1,1,1,1,1,1,1,1,1,1,1,1,1,1,1,
1,1,1,1,1,1,1,1,1,1,1,1,1,1,1,1,1,1,1,1,1,1,1,1,1,1,1,1,1,1,1,1,1,1,1,1,
1,1,1,1,1,1,1,1,1,1,1,1,1,1,1,1,1,1,1,1,1,1,1,1,1,1,1,1,1,1,1,1,1,1,1,1,
1,1,1,1,1,1,1,1,1,1,1,1,1,1,1,1,1,4),(0.,0.115296848757168),(11.6154215191109,
12.1154145856246,12.6154076521384,13.1154007186521,13.6153937851658,14.1153868516796,
14.6153799181933,15.1153729847071,15.6153660512208,16.1153591177345,16.6153521842483,
17.115345250762,17.6153383172757,18.1153313837895,18.6153244503032,19.1153175168169,
19.6153105833307,20.1153036498444,20.6152967163581,21.1152897828719,21.6152828493856,
22.1152759158993,22.6152689824131,23.1152620489268,23.6152551154406,24.1152481819543,
24.615241248468,25.1152343149818,25.6152273814955,26.1152204480092,26.615213514523,
27.1152065810367,27.6151996475504,28.1151927140642,28.6151857805779,29.1151788470916,
29.6151719136054,30.1151649801191,30.6151580466328,31.1151511131466,31.6151441796603,
32.115137246174,32.6151303126878,33.1151233792015,33.6151164457153,34.115109512229,
34.6151025787427,35.1150956452565,35.6150887117702,36.1150817782839,36.6150748447977,
37.1150679113114,37.6150609778251,38.1150540443389,38.6150471108526,39.1150401773663,
39.6150332438801,40.1150263103938,40.6150193769075,41.1150124434213,41.615005509935,
42.1149985764488,42.6149916429625,43.1149847094762,43.61497777599,44.1149708425037,
44.6149639090174,45.1149569755312,45.6149500420449,46.1149431085586,46.6149361750724,
47.1149292415861,47.6149223080998,48.1149153746136,48.6149084411273,49.114901507641,
49.6148945741548,50.1148876406685,50.6148807071823,51.114873773696,51.6148668402097,
52.1148599067235,52.6148529732372,53.1148460397509,53.6148391062647,54.1148321727784,
54.6148252392921,55.1148183058059,55.6148113723196,56.1148044388333,56.6147975053471,
57.1147905718608,57.6147836383745,58.1147767048883,58.614769771402,59.1147628379157,
59.6147559044295,60.1147489709432,60.6147420374569,61.1147351039707,61.6147281704844,
62.1147212369982,62.6147143035119,63.1147073700256,63.6147004365394,64.1146935030531,
64.6146865695668,65.1146796360806,65.6146727025943,66.114665769108,66.6146588356218,
67.1146519021355,67.6146449686492,68.114638035163,68.6146311016767,69.1146241681904,
69.6146172347042,70.1146103012179,70.6146033677317,71.1145964342454,71.6145895007591,
72.1145825672729,72.6145756337866,73.1145687003003,73.6145617668141,74.1145548333278,
74.6145478998415,75.1145409663553,75.614534032869,76.1145270993827,76.6145201658965,
77.1145132324102,77.614506298924,78.1144993654377,78.6144924319514,79.1144854984652,
79.6144785649789,80.1144716314926,80.6144646980064,81.1144577645201,81.6144508310338,
82.1144438975476,82.6144369640613,83.114430030575,83.6144230970888,84.1144161636025,
84.6144092301162,85.11440229663,85.6143953631437,86.1143884296575,86.6143814961712,
87.1143745626849,87.6143676291987,88.1143606957124,88.6143537622261,89.1143468287399,
89.6143398952536,90.1143329617673,90.6143260282811,91.1143190947948,91.6143121613085,
92.1143052278223,92.614298294336,93.1142913608497,93.6142844273635,94.1142774938772,
94.6142705603909,95.1142636269047,95.6142566934184,96.1142497599322,96.6142428264459,
97.1142358929596,97.6142289594734,98.1142220259871,98.6142150925008,99.1142081590146,
99.6142012255283,100.114194292042,100.614187358556,101.11418042507,101.614173491583,
102.114166558097,102.614159624611,103.114152691124,103.614145757638,104.114138824152,
104.614131890666,105.114124957179,105.614118023693,106.114111090207,106.614104156721,
107.114097223234,107.614090289748,108.114083356262,108.614076422776,109.114069489289,
109.614062555803,110.114055622317,110.61404868883,111.114041755344,111.614034821858,
112.114027888372,112.614020954885,113.114014021399,113.614007087913,114.114000154427,
114.61399322094,115.113986287454,115.613979353968,116.113972420482,116.613965486995,
117.113958553509,117.613951620023,118.113944686536,118.61393775305,119.113930819564,
119.613923886078,120.113916952591,120.613910019105,121.113903085619,121.613896152133,
122.113889218646,122.61388228516,123.113875351674,123.613868418188,124.113861484701,
124.613854551215,125.113847617729,125.613840684243,126.113833750756,126.61382681727,
127.113819883784,127.613812950297,128.113806016811,128.613799083325,129.113792149839,
129.613785216352,130.113778282866,130.61377134938,131.113764415894,131.613757482407,
132.113750548921,132.613743615435,133.113736681949,133.613729748462,134.113722814976,
134.61371588149,135.113708948003,135.613702014517,136.113695081031,136.613688147545,
137.113681214058,137.613674280572,138.113667347086,138.6136604136,139.113653480113,
139.613646546627,140.113639613141,140.613632679655,141.113625746168,141.613618812682,
142.113611879196,142.61360494571,143.113598012223,143.613591078737,144.113584145251,
144.613577211764,145.113570278278,145.613563344792,146.113556411306,146.613549477819,
147.113542544333,147.613535610847,148.113528677361,148.613521743874,149.113514810388,
149.613507876902,150.113500943416,150.613494009929,151.113487076443,151.613480142957,
152.11347320947,152.613466275984,153.113459342498,153.613452409012,154.113445475525,
154.613438542039,155.113431608553,155.613424675067,156.11341774158,156.613410808094,
157.113403874608,157.613396941122,158.113390007635,158.613383074149,159.113376140663,
159.613369207177,160.11336227369,160.613355340204,161.113348406718,161.613341473231,
162.113334539745,162.613327606259,163.113320672773,163.613313739286,164.1133068058,
164.613299872314,165.113292938828,165.613286005341,166.113279071855,166.613272138369,
167.113265204883,167.613258271396,168.11325133791,168.613244404424,169.113237470937,
169.613230537451,170.113223603965,170.613216670479,171.113209736992,171.613202803506,
172.11319587002,172.613188936534,173.113182003047,173.613175069561,174.113168136075,
174.613161202589,175.113154269102,175.613147335616,176.11314040213,176.613133468643,
177.113126535157,177.613119601671,178.113112668185,178.613105734698,179.113098801212,
179.613091867726,180.11308493424,180.613078000753,181.113071067267,181.613064133781,
182.113057200295,182.613050266808,183.113043333322,183.613036399836,184.11302946635,
184.613022532863,185.113015599377,185.613008665891,186.113001732404,186.612994798918,
187.112987865432,187.612980931946,188.112973998459,188.612967064973,189.112960131487,
189.612953198001,190.112946264514,190.612939331028,191.112932397542,191.612925464056,
192.112918530569,192.612911597083,193.112904663597,193.61289773011,194.112890796624,
194.612883863138,195.112876929652,195.612869996165,196.112863062679,196.612856129193,
197.112849195707,197.61284226222,198.112835328734,198.612828395248,199.112821461762,
199.612814528275,200.112807594789,200.612800661303,201.112793727816,201.61278679433,
202.112779860844,202.612772927358,203.112765993871,203.612759060385,204.112752126899,
204.612745193413,205.112738259926,205.61273132644,206.112724392954,206.612717459468,
207.112710525981,207.612703592495,208.112696659009,208.612689725523,209.112682792036,
209.61267585855,210.112668925064,210.612661991577,211.112655058091,211.612648124605,
212.112641191119,212.612634257632,213.112627324146,213.61262039066,214.112613457174,
214.612606523687,215.112599590201,215.612592656715,216.112585723229,216.612578789742,
217.112571856256,217.61256492277,218.112557989284,218.612551055797,219.112544122311,
219.612537188825,220.112530255338,220.612523321852,221.112516388366,221.61250945488,
222.112502521393,222.612495587907,223.112488654421,223.612481720935,224.112474787448,
224.612467853962,225.112460920476,225.61245398699,226.112447053503,226.612440120017,
227.112433186531,227.612426253044),.UNSPECIFIED.);
#254=B_SPLINE_SURFACE_WITH_KNOTS('',3,3,((#37108,#37109,#37110,#37111,#37112,
#37113,#37114,#37115,#37116,#37117,#37118,#37119,#37120,#37121,#37122,#37123,
#37124,#37125,#37126,#37127,#37128,#37129,#37130,#37131,#37132,#37133,#37134,
#37135,#37136,#37137,#37138,#37139,#37140,#37141,#37142,#37143,#37144,#37145,
#37146,#37147,#37148,#37149,#37150,#37151,#37152,#37153,#37154,#37155,#37156,
#37157,#37158,#37159,#37160,#37161,#37162,#37163,#37164,#37165,#37166,#37167,
#37168,#37169,#37170,#37171,#37172,#37173,#37174,#37175,#37176,#37177,#37178,
#37179,#37180,#37181,#37182,#37183,#37184,#37185,#37186,#37187,#37188,#37189,
#37190,#37191,#37192,#37193,#37194,#37195,#37196,#37197,#37198,#37199,#37200),
(#37201,#37202,#37203,#37204,#37205,#37206,#37207,#37208,#37209,#37210,
#37211,#37212,#37213,#37214,#37215,#37216,#37217,#37218,#37219,#37220,#37221,
#37222,#37223,#37224,#37225,#37226,#37227,#37228,#37229,#37230,#37231,#37232,
#37233,#37234,#37235,#37236,#37237,#37238,#37239,#37240,#37241,#37242,#37243,
#37244,#37245,#37246,#37247,#37248,#37249,#37250,#37251,#37252,#37253,#37254,
#37255,#37256,#37257,#37258,#37259,#37260,#37261,#37262,#37263,#37264,#37265,
#37266,#37267,#37268,#37269,#37270,#37271,#37272,#37273,#37274,#37275,#37276,
#37277,#37278,#37279,#37280,#37281,#37282,#37283,#37284,#37285,#37286,#37287,
#37288,#37289,#37290,#37291,#37292,#37293),(#37294,#37295,#37296,#37297,
#37298,#37299,#37300,#37301,#37302,#37303,#37304,#37305,#37306,#37307,#37308,
#37309,#37310,#37311,#37312,#37313,#37314,#37315,#37316,#37317,#37318,#37319,
#37320,#37321,#37322,#37323,#37324,#37325,#37326,#37327,#37328,#37329,#37330,
#37331,#37332,#37333,#37334,#37335,#37336,#37337,#37338,#37339,#37340,#37341,
#37342,#37343,#37344,#37345,#37346,#37347,#37348,#37349,#37350,#37351,#37352,
#37353,#37354,#37355,#37356,#37357,#37358,#37359,#37360,#37361,#37362,#37363,
#37364,#37365,#37366,#37367,#37368,#37369,#37370,#37371,#37372,#37373,#37374,
#37375,#37376,#37377,#37378,#37379,#37380,#37381,#37382,#37383,#37384,#37385,
#37386),(#37387,#37388,#37389,#37390,#37391,#37392,#37393,#37394,#37395,
#37396,#37397,#37398,#37399,#37400,#37401,#37402,#37403,#37404,#37405,#37406,
#37407,#37408,#37409,#37410,#37411,#37412,#37413,#37414,#37415,#37416,#37417,
#37418,#37419,#37420,#37421,#37422,#37423,#37424,#37425,#37426,#37427,#37428,
#37429,#37430,#37431,#37432,#37433,#37434,#37435,#37436,#37437,#37438,#37439,
#37440,#37441,#37442,#37443,#37444,#37445,#37446,#37447,#37448,#37449,#37450,
#37451,#37452,#37453,#37454,#37455,#37456,#37457,#37458,#37459,#37460,#37461,
#37462,#37463,#37464,#37465,#37466,#37467,#37468,#37469,#37470,#37471,#37472,
#37473,#37474,#37475,#37476,#37477,#37478,#37479)),.UNSPECIFIED.,.F.,.F.,
 .F.,(4,4),(4,1,1,1,1,1,1,1,1,1,1,1,1,1,1,1,1,1,1,1,1,1,1,1,1,1,1,1,1,1,
1,1,1,1,1,1,1,1,1,1,1,1,1,1,1,1,1,1,1,1,1,1,1,1,1,1,1,1,1,1,1,1,1,1,1,1,
1,1,1,1,1,1,1,1,1,1,1,1,1,1,1,1,1,1,1,1,1,1,1,1,4),(0.,0.0989001011121829),
(8.30505915324879,8.79698604421743,9.28891293518608,9.78083982615473,10.2727667171234,
10.764693608092,11.2566204990607,11.7485473900293,12.240474280998,12.7324011719666,
13.2243280629353,13.7162549539039,14.2081818448726,14.7001087358412,15.1920356268099,
15.6839625177785,16.1758894087472,16.6678162997158,17.1597431906845,17.6516700816531,
18.1435969726218,18.6355238635904,19.127450754559,19.6193776455277,20.1113045364963,
20.603231427465,21.0951583184336,21.5870852094023,22.0790121003709,22.5709389913396,
23.0628658823082,23.5547927732769,24.0467196642455,24.5386465552142,25.0305734461828,
25.5225003371515,26.0144272281201,26.5063541190888,26.9982810100574,27.4902079010261,
27.9821347919947,28.4740616829634,28.965988573932,29.4579154649007,29.9498423558693,
30.441769246838,30.9336961378066,31.4256230287753,31.9175499197439,32.4094768107125,
32.9014037016812,33.3933305926498,33.8852574836185,34.3771843745871,34.8691112655558,
35.3610381565244,35.8529650474931,36.3448919384617,36.8368188294304,37.328745720399,
37.8206726113677,38.3125995023363,38.804526393305,39.2964532842736,39.7883801752423,
40.2803070662109,40.7722339571796,41.2641608481482,41.7560877391169,42.2480146300855,
42.7399415210542,43.2318684120228,43.7237953029915,44.2157221939601,44.7076490849288,
45.1995759758974,45.6915028668661,46.1834297578347,46.6753566488034,47.167283539772,
47.6592104307407,48.1511373217093,48.6430642126779,49.1349911036466,49.6269179946152,
50.1188448855839,50.6107717765525,51.1026986675212,51.5946255584898,52.0865524494585,
52.5784793404271),.UNSPECIFIED.);
#255=B_SPLINE_SURFACE_WITH_KNOTS('',3,3,((#37895,#37896,#37897,#37898,#37899,
#37900,#37901,#37902,#37903,#37904,#37905,#37906,#37907,#37908,#37909,#37910,
#37911,#37912,#37913,#37914,#37915,#37916,#37917,#37918,#37919,#37920,#37921,
#37922,#37923,#37924,#37925,#37926,#37927,#37928,#37929,#37930,#37931,#37932,
#37933,#37934,#37935,#37936,#37937,#37938,#37939,#37940,#37941,#37942,#37943,
#37944,#37945,#37946,#37947,#37948,#37949,#37950,#37951,#37952,#37953,#37954,
#37955,#37956,#37957,#37958,#37959,#37960,#37961,#37962,#37963,#37964,#37965,
#37966,#37967,#37968,#37969,#37970,#37971,#37972,#37973,#37974,#37975,#37976,
#37977,#37978,#37979,#37980,#37981,#37982,#37983,#37984,#37985,#37986,#37987),
(#37988,#37989,#37990,#37991,#37992,#37993,#37994,#37995,#37996,#37997,
#37998,#37999,#38000,#38001,#38002,#38003,#38004,#38005,#38006,#38007,#38008,
#38009,#38010,#38011,#38012,#38013,#38014,#38015,#38016,#38017,#38018,#38019,
#38020,#38021,#38022,#38023,#38024,#38025,#38026,#38027,#38028,#38029,#38030,
#38031,#38032,#38033,#38034,#38035,#38036,#38037,#38038,#38039,#38040,#38041,
#38042,#38043,#38044,#38045,#38046,#38047,#38048,#38049,#38050,#38051,#38052,
#38053,#38054,#38055,#38056,#38057,#38058,#38059,#38060,#38061,#38062,#38063,
#38064,#38065,#38066,#38067,#38068,#38069,#38070,#38071,#38072,#38073,#38074,
#38075,#38076,#38077,#38078,#38079,#38080),(#38081,#38082,#38083,#38084,
#38085,#38086,#38087,#38088,#38089,#38090,#38091,#38092,#38093,#38094,#38095,
#38096,#38097,#38098,#38099,#38100,#38101,#38102,#38103,#38104,#38105,#38106,
#38107,#38108,#38109,#38110,#38111,#38112,#38113,#38114,#38115,#38116,#38117,
#38118,#38119,#38120,#38121,#38122,#38123,#38124,#38125,#38126,#38127,#38128,
#38129,#38130,#38131,#38132,#38133,#38134,#38135,#38136,#38137,#38138,#38139,
#38140,#38141,#38142,#38143,#38144,#38145,#38146,#38147,#38148,#38149,#38150,
#38151,#38152,#38153,#38154,#38155,#38156,#38157,#38158,#38159,#38160,#38161,
#38162,#38163,#38164,#38165,#38166,#38167,#38168,#38169,#38170,#38171,#38172,
#38173),(#38174,#38175,#38176,#38177,#38178,#38179,#38180,#38181,#38182,
#38183,#38184,#38185,#38186,#38187,#38188,#38189,#38190,#38191,#38192,#38193,
#38194,#38195,#38196,#38197,#38198,#38199,#38200,#38201,#38202,#38203,#38204,
#38205,#38206,#38207,#38208,#38209,#38210,#38211,#38212,#38213,#38214,#38215,
#38216,#38217,#38218,#38219,#38220,#38221,#38222,#38223,#38224,#38225,#38226,
#38227,#38228,#38229,#38230,#38231,#38232,#38233,#38234,#38235,#38236,#38237,
#38238,#38239,#38240,#38241,#38242,#38243,#38244,#38245,#38246,#38247,#38248,
#38249,#38250,#38251,#38252,#38253,#38254,#38255,#38256,#38257,#38258,#38259,
#38260,#38261,#38262,#38263,#38264,#38265,#38266)),.UNSPECIFIED.,.F.,.F.,
 .F.,(4,4),(4,1,1,1,1,1,1,1,1,1,1,1,1,1,1,1,1,1,1,1,1,1,1,1,1,1,1,1,1,1,
1,1,1,1,1,1,1,1,1,1,1,1,1,1,1,1,1,1,1,1,1,1,1,1,1,1,1,1,1,1,1,1,1,1,1,1,
1,1,1,1,1,1,1,1,1,1,1,1,1,1,1,1,1,1,1,1,1,1,1,1,4),(0.,0.0989001011121829),
(11.6147305479243,12.1066574388929,12.5985843298616,13.0905112208302,13.5824381117989,
14.0743650027675,14.5662918937362,15.0582187847048,15.5501456756735,16.0420725666421,
16.5339994576108,17.0259263485794,17.5178532395481,18.0097801305167,18.5017070214854,
18.993633912454,19.4855608034226,19.9774876943913,20.4694145853599,20.9613414763286,
21.4532683672972,21.9451952582659,22.4371221492345,22.9290490402032,23.4209759311718,
23.9129028221405,24.4048297131091,24.8967566040778,25.3886834950464,25.8806103860151,
26.3725372769837,26.8644641679524,27.356391058921,27.8483179498897,28.3402448408583,
28.832171731827,29.3240986227956,29.8160255137643,30.3079524047329,30.7998792957016,
31.2918061866702,31.7837330776389,32.2756599686075,32.7675868595761,33.2595137505448,
33.7514406415134,34.2433675324821,34.7352944234507,35.2272213144194,35.719148205388,
36.2110750963567,36.7030019873253,37.194928878294,37.6868557692626,38.1787826602313,
38.6707095511999,39.1626364421686,39.6545633331372,40.1464902241059,40.6384171150745,
41.1303440060432,41.6222708970118,42.1141977879805,42.6061246789491,43.0980515699178,
43.5899784608864,44.0819053518551,44.5738322428237,45.0657591337924,45.557686024761,
46.0496129157297,46.5415398066983,47.033466697667,47.5253935886356,48.0173204796042,
48.5092473705729,49.0011742615415,49.4931011525102,49.9850280434788,50.4769549344475,
50.9688818254161,51.4608087163848,51.9527356073534,52.4446624983221,52.9365893892907,
53.4285162802594,53.920443171228,54.4123700621967,54.9042969531653,55.396223844134,
55.8881507351026),.UNSPECIFIED.);
#256=TOROIDAL_SURFACE('',#15366,60.5,2.);
#257=TOROIDAL_SURFACE('',#15369,12.,2.);
#258=TOROIDAL_SURFACE('',#15373,60.5,2.);
#259=TOROIDAL_SURFACE('',#15374,12.,2.);
#260=TOROIDAL_SURFACE('',#15383,60.5,2.);
#261=TOROIDAL_SURFACE('',#15387,12.,2.);
#262=TOROIDAL_SURFACE('',#15394,60.5,2.);
#263=TOROIDAL_SURFACE('',#15398,12.,2.);
#264=TOROIDAL_SURFACE('',#15402,48.8,2.);
#265=TOROIDAL_SURFACE('',#15409,26.,2.);
#266=TOROIDAL_SURFACE('',#15415,26.,2.);
#267=TOROIDAL_SURFACE('',#15425,26.,2.);
#268=TOROIDAL_SURFACE('',#15433,26.,2.);
#269=TOROIDAL_SURFACE('',#15442,26.,2.);
#270=TOROIDAL_SURFACE('',#15447,26.,2.);
#271=TOROIDAL_SURFACE('',#15452,26.,2.);
#272=TOROIDAL_SURFACE('',#15457,26.,2.);
#273=TOROIDAL_SURFACE('',#15461,52.,2.);
#274=TOROIDAL_SURFACE('',#15563,12.,2.);
#275=TOROIDAL_SURFACE('',#15654,45.05,2.);
#276=TOROIDAL_SURFACE('',#15660,26.,2.);
#277=TOROIDAL_SURFACE('',#15665,26.,2.);
#278=TOROIDAL_SURFACE('',#15671,26.,2.);
#279=TOROIDAL_SURFACE('',#15678,26.,2.);
#280=TOROIDAL_SURFACE('',#15684,26.,2.);
#281=TOROIDAL_SURFACE('',#15692,26.,2.);
#282=TOROIDAL_SURFACE('',#15703,26.,2.);
#283=TOROIDAL_SURFACE('',#15704,26.,2.);
#284=TOROIDAL_SURFACE('',#15710,26.,2.);
#285=TOROIDAL_SURFACE('',#15716,26.,2.);
#286=TOROIDAL_SURFACE('',#15725,12.,2.);
#287=TOROIDAL_SURFACE('',#15738,12.,2.);
#288=TOROIDAL_SURFACE('',#15756,26.,2.);
#289=TOROIDAL_SURFACE('',#15760,26.,2.);
#290=TOROIDAL_SURFACE('',#15763,12.,2.);
#291=TOROIDAL_SURFACE('',#15766,26.,2.);
#292=TOROIDAL_SURFACE('',#15772,26.,2.);
#293=ELLIPSE('',#15321,13.946906437048,2.);
#294=ELLIPSE('',#15324,13.946906437048,2.);
#295=ELLIPSE('',#15327,13.946906437048,2.);
#296=ELLIPSE('',#15331,13.946906437048,2.);
#297=ELLIPSE('',#15340,13.946906437048,2.);
#298=ELLIPSE('',#15343,13.946906437048,2.);
#299=ELLIPSE('',#15346,13.946906437048,2.);
#300=ELLIPSE('',#15350,13.946906437048,2.);
#301=ELLIPSE('',#15801,67.8822509939087,48.);
#302=ELLIPSE('',#15802,67.8822509939087,48.);
#303=ELLIPSE('',#15806,67.8822509939087,48.);
#304=ELLIPSE('',#15807,71.3756226163554,48.);
#305=ELLIPSE('',#15808,50.4701867634368,48.);
#306=ELLIPSE('',#15809,71.3756226163554,48.);
#307=ELLIPSE('',#15811,71.3756226163554,48.);
#308=ELLIPSE('',#15813,50.4701867634368,48.);
#309=ELLIPSE('',#15814,21.0292444847653,20.);
#310=ELLIPSE('',#15816,67.8822509939087,48.);
#311=ELLIPSE('',#15821,71.3756226163554,48.);
#312=ELLIPSE('',#15842,17.6918116652872,12.51);
#313=ELLIPSE('',#15844,17.6918116652872,12.51);
#314=ELLIPSE('',#15849,17.6918116652872,12.51);
#315=ELLIPSE('',#15851,17.6918116652879,12.51);
#316=ELLIPSE('',#15903,32.5269119345808,23.);
#317=ELLIPSE('',#15904,46.6690475583115,33.);
#318=ELLIPSE('',#15907,46.6690475583112,33.);
#319=ELLIPSE('',#15908,32.5269119345805,23.);
#320=ELLIPSE('',#15910,46.6690475583115,33.);
#321=ELLIPSE('',#15911,32.5269119345807,23.);
#322=ELLIPSE('',#15914,32.5269119345808,23.);
#323=ELLIPSE('',#15915,46.6690475583116,33.);
#324=ELLIPSE('',#15917,32.5269119345811,23.);
#325=ELLIPSE('',#15918,46.669047558312,33.);
#326=ELLIPSE('',#15921,46.669047558312,33.);
#327=ELLIPSE('',#15922,32.5269119345811,23.);
#328=ELLIPSE('',#15924,46.6690475583117,33.);
#329=ELLIPSE('',#15925,32.5269119345809,23.);
#330=ELLIPSE('',#15928,32.5269119345811,23.);
#331=ELLIPSE('',#15929,46.669047558312,33.);
#332=(
BOUNDED_CURVE()
B_SPLINE_CURVE(2,(#21090,#21091,#21092),.UNSPECIFIED.,.F.,.F.)
B_SPLINE_CURVE_WITH_KNOTS((3,3),(-9.16934047811363,-8.99429341935052),
 .UNSPECIFIED.)
CURVE()
GEOMETRIC_REPRESENTATION_ITEM()
RATIONAL_B_SPLINE_CURVE((1.20544110146931,1.20730170334354,1.20901639344262))
REPRESENTATION_ITEM('')
);
#333=(
BOUNDED_CURVE()
B_SPLINE_CURVE(2,(#21112,#21113,#21114),.UNSPECIFIED.,.F.,.F.)
B_SPLINE_CURVE_WITH_KNOTS((3,3),(-4.88014350616112,-4.705096447398),
 .UNSPECIFIED.)
CURVE()
GEOMETRIC_REPRESENTATION_ITEM()
RATIONAL_B_SPLINE_CURVE((1.20901639344263,1.20730170334354,1.20544110146931))
REPRESENTATION_ITEM('')
);
#334=(
BOUNDED_CURVE()
B_SPLINE_CURVE(2,(#21198,#21199,#21200),.UNSPECIFIED.,.F.,.F.)
B_SPLINE_CURVE_WITH_KNOTS((3,3),(-4.88014350616107,-4.70509644739795),
 .UNSPECIFIED.)
CURVE()
GEOMETRIC_REPRESENTATION_ITEM()
RATIONAL_B_SPLINE_CURVE((1.20901639344262,1.20730170334354,1.20544110146931))
REPRESENTATION_ITEM('')
);
#335=(
BOUNDED_CURVE()
B_SPLINE_CURVE(2,(#21291,#21292,#21293),.UNSPECIFIED.,.F.,.F.)
B_SPLINE_CURVE_WITH_KNOTS((3,3),(-9.16934047811369,-8.99429341935056),
 .UNSPECIFIED.)
CURVE()
GEOMETRIC_REPRESENTATION_ITEM()
RATIONAL_B_SPLINE_CURVE((1.20544110146931,1.20730170334354,1.20901639344263))
REPRESENTATION_ITEM('')
);
#336=(
BOUNDED_CURVE()
B_SPLINE_CURVE(3,(#24045,#24046,#24047,#24048,#24049,#24050),
 .UNSPECIFIED.,.F.,.F.)
B_SPLINE_CURVE_WITH_KNOTS((4,2,4),(0.,0.00123256806504644,0.00166298225708981),
 .UNSPECIFIED.)
CURVE()
GEOMETRIC_REPRESENTATION_ITEM()
RATIONAL_B_SPLINE_CURVE((1.,1.,1.,1.,1.,1.))
REPRESENTATION_ITEM('')
);
#337=(
BOUNDED_CURVE()
B_SPLINE_CURVE(3,(#24056,#24057,#24058,#24059,#24060,#24061),
 .UNSPECIFIED.,.F.,.F.)
B_SPLINE_CURVE_WITH_KNOTS((4,2,4),(-0.00166298225712823,-0.00123256806504644,
0.),.UNSPECIFIED.)
CURVE()
GEOMETRIC_REPRESENTATION_ITEM()
RATIONAL_B_SPLINE_CURVE((1.,1.,1.,1.,1.,1.))
REPRESENTATION_ITEM('')
);
#338=(
BOUNDED_CURVE()
B_SPLINE_CURVE(2,(#25747,#25748,#25749),.UNSPECIFIED.,.F.,.F.)
B_SPLINE_CURVE_WITH_KNOTS((3,3),(0.00089915875038223,0.119861415155793),
 .UNSPECIFIED.)
CURVE()
GEOMETRIC_REPRESENTATION_ITEM()
RATIONAL_B_SPLINE_CURVE((1.00000690885838,1.00046048906391,1.))
REPRESENTATION_ITEM('')
);
#339=(
BOUNDED_CURVE()
B_SPLINE_CURVE(2,(#25761,#25762,#25763),.UNSPECIFIED.,.F.,.F.)
B_SPLINE_CURVE_WITH_KNOTS((3,3),(0.,0.118962256406331),.UNSPECIFIED.)
CURVE()
GEOMETRIC_REPRESENTATION_ITEM()
RATIONAL_B_SPLINE_CURVE((1.,1.00046048906569,1.0000069088584))
REPRESENTATION_ITEM('')
);
#340=(
BOUNDED_CURVE()
B_SPLINE_CURVE(2,(#25773,#25774,#25775),.UNSPECIFIED.,.F.,.F.)
B_SPLINE_CURVE_WITH_KNOTS((3,3),(-47.8696729569845,-47.8687190848821),
 .UNSPECIFIED.)
CURVE()
GEOMETRIC_REPRESENTATION_ITEM()
RATIONAL_B_SPLINE_CURVE((15.2054806811783,15.2077824060813,15.2100840336135))
REPRESENTATION_ITEM('')
);
#341=(
BOUNDED_CURVE()
B_SPLINE_CURVE(2,(#25778,#25779,#25780),.UNSPECIFIED.,.F.,.F.)
B_SPLINE_CURVE_WITH_KNOTS((3,3),(-2.77393487400909,-2.77298100190668),
 .UNSPECIFIED.)
CURVE()
GEOMETRIC_REPRESENTATION_ITEM()
RATIONAL_B_SPLINE_CURVE((15.2100840336134,15.2077824060812,15.2054806811782))
REPRESENTATION_ITEM('')
);
#342=(
BOUNDED_CURVE()
B_SPLINE_CURVE(2,(#25790,#25791,#25792),.UNSPECIFIED.,.F.,.F.)
B_SPLINE_CURVE_WITH_KNOTS((3,3),(0.111140514111159,0.111966209987666),
 .UNSPECIFIED.)
CURVE()
GEOMETRIC_REPRESENTATION_ITEM()
RATIONAL_B_SPLINE_CURVE((1.00000394455129,1.00000198692827,1.))
REPRESENTATION_ITEM('')
);
#343=(
BOUNDED_CURVE()
B_SPLINE_CURVE(2,(#25799,#25800,#25801),.UNSPECIFIED.,.F.,.F.)
B_SPLINE_CURVE_WITH_KNOTS((3,3),(0.,0.000825695876467816),.UNSPECIFIED.)
CURVE()
GEOMETRIC_REPRESENTATION_ITEM()
RATIONAL_B_SPLINE_CURVE((1.,1.00000198692868,1.00000394455211))
REPRESENTATION_ITEM('')
);
#344=(
BOUNDED_CURVE()
B_SPLINE_CURVE(2,(#25812,#25813,#25814),.UNSPECIFIED.,.F.,.F.)
B_SPLINE_CURVE_WITH_KNOTS((3,3),(0.000899158750379295,0.119861415155793),
 .UNSPECIFIED.)
CURVE()
GEOMETRIC_REPRESENTATION_ITEM()
RATIONAL_B_SPLINE_CURVE((1.00000690885842,1.00046048906656,1.))
REPRESENTATION_ITEM('')
);
#345=(
BOUNDED_CURVE()
B_SPLINE_CURVE(2,(#25826,#25827,#25828),.UNSPECIFIED.,.F.,.F.)
B_SPLINE_CURVE_WITH_KNOTS((3,3),(0.,0.11896225640633),.UNSPECIFIED.)
CURVE()
GEOMETRIC_REPRESENTATION_ITEM()
RATIONAL_B_SPLINE_CURVE((1.,1.00046048906395,1.00000690885837))
REPRESENTATION_ITEM('')
);
#346=(
BOUNDED_CURVE()
B_SPLINE_CURVE(2,(#25838,#25839,#25840),.UNSPECIFIED.,.F.,.F.)
B_SPLINE_CURVE_WITH_KNOTS((3,3),(-47.8696729569843,-47.8687190848819),
 .UNSPECIFIED.)
CURVE()
GEOMETRIC_REPRESENTATION_ITEM()
RATIONAL_B_SPLINE_CURVE((15.2054806811781,15.2077824060811,15.2100840336132))
REPRESENTATION_ITEM('')
);
#347=(
BOUNDED_CURVE()
B_SPLINE_CURVE(2,(#25843,#25844,#25845),.UNSPECIFIED.,.F.,.F.)
B_SPLINE_CURVE_WITH_KNOTS((3,3),(-2.77393487400938,-2.77298100190697),
 .UNSPECIFIED.)
CURVE()
GEOMETRIC_REPRESENTATION_ITEM()
RATIONAL_B_SPLINE_CURVE((15.2100840336132,15.2077824060811,15.2054806811781))
REPRESENTATION_ITEM('')
);
#348=(
BOUNDED_CURVE()
B_SPLINE_CURVE(2,(#25855,#25856,#25857),.UNSPECIFIED.,.F.,.F.)
B_SPLINE_CURVE_WITH_KNOTS((3,3),(0.111140514109634,0.111966209987666),
 .UNSPECIFIED.)
CURVE()
GEOMETRIC_REPRESENTATION_ITEM()
RATIONAL_B_SPLINE_CURVE((1.00000394455479,1.00000198693003,1.))
REPRESENTATION_ITEM('')
);
#349=(
BOUNDED_CURVE()
B_SPLINE_CURVE(2,(#25864,#25865,#25866),.UNSPECIFIED.,.F.,.F.)
B_SPLINE_CURVE_WITH_KNOTS((3,3),(0.,0.000825695875370319),.UNSPECIFIED.)
CURVE()
GEOMETRIC_REPRESENTATION_ITEM()
RATIONAL_B_SPLINE_CURVE((1.,1.00000198692765,1.00000394455006))
REPRESENTATION_ITEM('')
);
#350=(
BOUNDED_CURVE()
B_SPLINE_CURVE(2,(#25877,#25878,#25879),.UNSPECIFIED.,.F.,.F.)
B_SPLINE_CURVE_WITH_KNOTS((3,3),(0.000899158750382334,0.119861415155793),
 .UNSPECIFIED.)
CURVE()
GEOMETRIC_REPRESENTATION_ITEM()
RATIONAL_B_SPLINE_CURVE((1.00000690885837,1.00046048906313,1.))
REPRESENTATION_ITEM('')
);
#351=(
BOUNDED_CURVE()
B_SPLINE_CURVE(2,(#25891,#25892,#25893),.UNSPECIFIED.,.F.,.F.)
B_SPLINE_CURVE_WITH_KNOTS((3,3),(0.,0.11896225640633),.UNSPECIFIED.)
CURVE()
GEOMETRIC_REPRESENTATION_ITEM()
RATIONAL_B_SPLINE_CURVE((1.,1.00046048906413,1.00000690885838))
REPRESENTATION_ITEM('')
);
#352=(
BOUNDED_CURVE()
B_SPLINE_CURVE(2,(#25903,#25904,#25905),.UNSPECIFIED.,.F.,.F.)
B_SPLINE_CURVE_WITH_KNOTS((3,3),(-47.8696729569845,-47.8687190848821),
 .UNSPECIFIED.)
CURVE()
GEOMETRIC_REPRESENTATION_ITEM()
RATIONAL_B_SPLINE_CURVE((15.2054806811782,15.2077824060812,15.2100840336134))
REPRESENTATION_ITEM('')
);
#353=(
BOUNDED_CURVE()
B_SPLINE_CURVE(2,(#25908,#25909,#25910),.UNSPECIFIED.,.F.,.F.)
B_SPLINE_CURVE_WITH_KNOTS((3,3),(-2.77393487400914,-2.77298100190673),
 .UNSPECIFIED.)
CURVE()
GEOMETRIC_REPRESENTATION_ITEM()
RATIONAL_B_SPLINE_CURVE((15.2100840336134,15.2077824060812,15.2054806811782))
REPRESENTATION_ITEM('')
);
#354=(
BOUNDED_CURVE()
B_SPLINE_CURVE(2,(#25920,#25921,#25922),.UNSPECIFIED.,.F.,.F.)
B_SPLINE_CURVE_WITH_KNOTS((3,3),(0.111140514110888,0.111966209987666),
 .UNSPECIFIED.)
CURVE()
GEOMETRIC_REPRESENTATION_ITEM()
RATIONAL_B_SPLINE_CURVE((1.000003944553,1.00000198692913,1.))
REPRESENTATION_ITEM('')
);
#355=(
BOUNDED_CURVE()
B_SPLINE_CURVE(2,(#25929,#25930,#25931),.UNSPECIFIED.,.F.,.F.)
B_SPLINE_CURVE_WITH_KNOTS((3,3),(0.,0.000825695876921701),.UNSPECIFIED.)
CURVE()
GEOMETRIC_REPRESENTATION_ITEM()
RATIONAL_B_SPLINE_CURVE((1.,1.0000019869287,1.00000394455216))
REPRESENTATION_ITEM('')
);
#356=(
BOUNDED_CURVE()
B_SPLINE_CURVE(2,(#25942,#25943,#25944),.UNSPECIFIED.,.F.,.F.)
B_SPLINE_CURVE_WITH_KNOTS((3,3),(0.000899158750381089,0.119861415155793),
 .UNSPECIFIED.)
CURVE()
GEOMETRIC_REPRESENTATION_ITEM()
RATIONAL_B_SPLINE_CURVE((1.00000690885838,1.00046048906409,1.))
REPRESENTATION_ITEM('')
);
#357=(
BOUNDED_CURVE()
B_SPLINE_CURVE(2,(#25956,#25957,#25958),.UNSPECIFIED.,.F.,.F.)
B_SPLINE_CURVE_WITH_KNOTS((3,3),(0.,0.118962256406332),.UNSPECIFIED.)
CURVE()
GEOMETRIC_REPRESENTATION_ITEM()
RATIONAL_B_SPLINE_CURVE((1.,1.00046048906654,1.00000690885841))
REPRESENTATION_ITEM('')
);
#358=(
BOUNDED_CURVE()
B_SPLINE_CURVE(2,(#25968,#25969,#25970),.UNSPECIFIED.,.F.,.F.)
B_SPLINE_CURVE_WITH_KNOTS((3,3),(-47.8696729569844,-47.868719084882),
 .UNSPECIFIED.)
CURVE()
GEOMETRIC_REPRESENTATION_ITEM()
RATIONAL_B_SPLINE_CURVE((15.2054806811782,15.2077824060812,15.2100840336134))
REPRESENTATION_ITEM('')
);
#359=(
BOUNDED_CURVE()
B_SPLINE_CURVE(2,(#25973,#25974,#25975),.UNSPECIFIED.,.F.,.F.)
B_SPLINE_CURVE_WITH_KNOTS((3,3),(-2.77393487400941,-2.772981001907),
 .UNSPECIFIED.)
CURVE()
GEOMETRIC_REPRESENTATION_ITEM()
RATIONAL_B_SPLINE_CURVE((15.2100840336131,15.207782406081,15.205480681178))
REPRESENTATION_ITEM('')
);
#360=(
BOUNDED_CURVE()
B_SPLINE_CURVE(2,(#25985,#25986,#25987),.UNSPECIFIED.,.F.,.F.)
B_SPLINE_CURVE_WITH_KNOTS((3,3),(0.111140514110977,0.111966209987666),
 .UNSPECIFIED.)
CURVE()
GEOMETRIC_REPRESENTATION_ITEM()
RATIONAL_B_SPLINE_CURVE((1.00000394455159,1.00000198692842,1.))
REPRESENTATION_ITEM('')
);
#361=(
BOUNDED_CURVE()
B_SPLINE_CURVE(2,(#25994,#25995,#25996),.UNSPECIFIED.,.F.,.F.)
B_SPLINE_CURVE_WITH_KNOTS((3,3),(0.,0.000825695874631881),.UNSPECIFIED.)
CURVE()
GEOMETRIC_REPRESENTATION_ITEM()
RATIONAL_B_SPLINE_CURVE((1.,1.00000198692687,1.00000394454852))
REPRESENTATION_ITEM('')
);
#362=(
BOUNDED_CURVE()
B_SPLINE_CURVE(2,(#26005,#26006,#26007),.UNSPECIFIED.,.F.,.F.)
B_SPLINE_CURVE_WITH_KNOTS((3,3),(0.000899158750383316,0.119861415155793),
 .UNSPECIFIED.)
CURVE()
GEOMETRIC_REPRESENTATION_ITEM()
RATIONAL_B_SPLINE_CURVE((1.00000690885837,1.00046048906313,1.))
REPRESENTATION_ITEM('')
);
#363=(
BOUNDED_CURVE()
B_SPLINE_CURVE(2,(#26011,#26012,#26013),.UNSPECIFIED.,.F.,.F.)
B_SPLINE_CURVE_WITH_KNOTS((3,3),(1.83887863060053,1.88690815084928),
 .UNSPECIFIED.)
CURVE()
GEOMETRIC_REPRESENTATION_ITEM()
RATIONAL_B_SPLINE_CURVE((1.02805437145288,1.01439356064084,1.))
REPRESENTATION_ITEM('')
);
#364=(
BOUNDED_CURVE()
B_SPLINE_CURVE(2,(#26017,#26018,#26019),.UNSPECIFIED.,.F.,.F.)
B_SPLINE_CURVE_WITH_KNOTS((3,3),(0.0704444719086716,0.0709678248042913),
 .UNSPECIFIED.)
CURVE()
GEOMETRIC_REPRESENTATION_ITEM()
RATIONAL_B_SPLINE_CURVE((1.00000394455158,1.00000198692841,1.))
REPRESENTATION_ITEM('')
);
#365=(
BOUNDED_CURVE()
B_SPLINE_CURVE(2,(#26028,#26029,#26030),.UNSPECIFIED.,.F.,.F.)
B_SPLINE_CURVE_WITH_KNOTS((3,3),(0.111140514109306,0.111966209987666),
 .UNSPECIFIED.)
CURVE()
GEOMETRIC_REPRESENTATION_ITEM()
RATIONAL_B_SPLINE_CURVE((1.00000394455327,1.00000198692926,1.))
REPRESENTATION_ITEM('')
);
#366=(
BOUNDED_CURVE()
B_SPLINE_CURVE(2,(#26036,#26037,#26038),.UNSPECIFIED.,.F.,.F.)
B_SPLINE_CURVE_WITH_KNOTS((3,3),(0.,0.118962256406332),.UNSPECIFIED.)
CURVE()
GEOMETRIC_REPRESENTATION_ITEM()
RATIONAL_B_SPLINE_CURVE((1.,1.00046048906504,1.00000690885839))
REPRESENTATION_ITEM('')
);
#367=(
BOUNDED_CURVE()
B_SPLINE_CURVE(2,(#26049,#26050,#26051),.UNSPECIFIED.,.F.,.F.)
B_SPLINE_CURVE_WITH_KNOTS((3,3),(-47.8696729569846,-47.8687190848822),
 .UNSPECIFIED.)
CURVE()
GEOMETRIC_REPRESENTATION_ITEM()
RATIONAL_B_SPLINE_CURVE((15.2054806811784,15.2077824060813,15.2100840336135))
REPRESENTATION_ITEM('')
);
#368=(
BOUNDED_CURVE()
B_SPLINE_CURVE(2,(#26054,#26055,#26056),.UNSPECIFIED.,.F.,.F.)
B_SPLINE_CURVE_WITH_KNOTS((3,3),(0.,0.000825695876215709),.UNSPECIFIED.)
CURVE()
GEOMETRIC_REPRESENTATION_ITEM()
RATIONAL_B_SPLINE_CURVE((1.,1.00000198692775,1.00000394455027))
REPRESENTATION_ITEM('')
);
#369=(
BOUNDED_CURVE()
B_SPLINE_CURVE(2,(#26068,#26069,#26070),.UNSPECIFIED.,.F.,.F.)
B_SPLINE_CURVE_WITH_KNOTS((3,3),(0.000899158750381245,0.119861415155792),
 .UNSPECIFIED.)
CURVE()
GEOMETRIC_REPRESENTATION_ITEM()
RATIONAL_B_SPLINE_CURVE((1.00000690885837,1.00046048906334,1.))
REPRESENTATION_ITEM('')
);
#370=(
BOUNDED_CURVE()
B_SPLINE_CURVE(2,(#26072,#26073,#26074),.UNSPECIFIED.,.F.,.F.)
B_SPLINE_CURVE_WITH_KNOTS((3,3),(0.111140514111096,0.111966209987666),
 .UNSPECIFIED.)
CURVE()
GEOMETRIC_REPRESENTATION_ITEM()
RATIONAL_B_SPLINE_CURVE((1.00000394455331,1.00000198692928,1.))
REPRESENTATION_ITEM('')
);
#371=(
BOUNDED_CURVE()
B_SPLINE_CURVE(2,(#26158,#26159,#26160),.UNSPECIFIED.,.F.,.F.)
B_SPLINE_CURVE_WITH_KNOTS((3,3),(0.,0.118962256406332),.UNSPECIFIED.)
CURVE()
GEOMETRIC_REPRESENTATION_ITEM()
RATIONAL_B_SPLINE_CURVE((1.,1.00046048906488,1.00000690885839))
REPRESENTATION_ITEM('')
);
#372=(
BOUNDED_CURVE()
B_SPLINE_CURVE(2,(#26169,#26170,#26171),.UNSPECIFIED.,.F.,.F.)
B_SPLINE_CURVE_WITH_KNOTS((3,3),(-47.8696729569843,-47.8687190848819),
 .UNSPECIFIED.)
CURVE()
GEOMETRIC_REPRESENTATION_ITEM()
RATIONAL_B_SPLINE_CURVE((15.2054806811781,15.2077824060811,15.2100840336132))
REPRESENTATION_ITEM('')
);
#373=(
BOUNDED_CURVE()
B_SPLINE_CURVE(2,(#26174,#26175,#26176),.UNSPECIFIED.,.F.,.F.)
B_SPLINE_CURVE_WITH_KNOTS((3,3),(-2.77393487400923,-2.77298100190682),
 .UNSPECIFIED.)
CURVE()
GEOMETRIC_REPRESENTATION_ITEM()
RATIONAL_B_SPLINE_CURVE((15.2100840336133,15.2077824060812,15.2054806811782))
REPRESENTATION_ITEM('')
);
#374=(
BOUNDED_CURVE()
B_SPLINE_CURVE(2,(#26191,#26192,#26193),.UNSPECIFIED.,.F.,.F.)
B_SPLINE_CURVE_WITH_KNOTS((3,3),(0.,0.0008256958761486),.UNSPECIFIED.)
CURVE()
GEOMETRIC_REPRESENTATION_ITEM()
RATIONAL_B_SPLINE_CURVE((1.,1.00000198692878,1.00000394455231))
REPRESENTATION_ITEM('')
);
#375=(
BOUNDED_CURVE()
B_SPLINE_CURVE(2,(#26203,#26204,#26205),.UNSPECIFIED.,.F.,.F.)
B_SPLINE_CURVE_WITH_KNOTS((3,3),(0.000899158750380169,0.119861415155792),
 .UNSPECIFIED.)
CURVE()
GEOMETRIC_REPRESENTATION_ITEM()
RATIONAL_B_SPLINE_CURVE((1.0000069088584,1.00046048906499,1.))
REPRESENTATION_ITEM('')
);
#376=(
BOUNDED_CURVE()
B_SPLINE_CURVE(2,(#26212,#26213,#26214),.UNSPECIFIED.,.F.,.F.)
B_SPLINE_CURVE_WITH_KNOTS((3,3),(0.,0.118962256406331),.UNSPECIFIED.)
CURVE()
GEOMETRIC_REPRESENTATION_ITEM()
RATIONAL_B_SPLINE_CURVE((1.,1.00046048906418,1.00000690885838))
REPRESENTATION_ITEM('')
);
#377=(
BOUNDED_CURVE()
B_SPLINE_CURVE(2,(#26223,#26224,#26225),.UNSPECIFIED.,.F.,.F.)
B_SPLINE_CURVE_WITH_KNOTS((3,3),(-47.8696729569847,-47.8687190848823),
 .UNSPECIFIED.)
CURVE()
GEOMETRIC_REPRESENTATION_ITEM()
RATIONAL_B_SPLINE_CURVE((15.2054806811785,15.2077824060814,15.2100840336136))
REPRESENTATION_ITEM('')
);
#378=(
BOUNDED_CURVE()
B_SPLINE_CURVE(2,(#26228,#26229,#26230),.UNSPECIFIED.,.F.,.F.)
B_SPLINE_CURVE_WITH_KNOTS((3,3),(-2.77393487400886,-2.77298100190645),
 .UNSPECIFIED.)
CURVE()
GEOMETRIC_REPRESENTATION_ITEM()
RATIONAL_B_SPLINE_CURVE((15.2100840336136,15.2077824060815,15.2054806811785))
REPRESENTATION_ITEM('')
);
#379=(
BOUNDED_CURVE()
B_SPLINE_CURVE(2,(#26240,#26241,#26242),.UNSPECIFIED.,.F.,.F.)
B_SPLINE_CURVE_WITH_KNOTS((3,3),(0.111140514112235,0.111966209987666),
 .UNSPECIFIED.)
CURVE()
GEOMETRIC_REPRESENTATION_ITEM()
RATIONAL_B_SPLINE_CURVE((1.00000394455079,1.00000198692802,1.))
REPRESENTATION_ITEM('')
);
#380=(
BOUNDED_CURVE()
B_SPLINE_CURVE(2,(#26249,#26250,#26251),.UNSPECIFIED.,.F.,.F.)
B_SPLINE_CURVE_WITH_KNOTS((3,3),(0.,0.000825695876969575),.UNSPECIFIED.)
CURVE()
GEOMETRIC_REPRESENTATION_ITEM()
RATIONAL_B_SPLINE_CURVE((1.,1.00000198692876,1.00000394455228))
REPRESENTATION_ITEM('')
);
#381=(
BOUNDED_CURVE()
B_SPLINE_CURVE(2,(#26365,#26366,#26367),.UNSPECIFIED.,.F.,.F.)
B_SPLINE_CURVE_WITH_KNOTS((3,3),(0.000899158750381918,0.119861415155793),
 .UNSPECIFIED.)
CURVE()
GEOMETRIC_REPRESENTATION_ITEM()
RATIONAL_B_SPLINE_CURVE((1.00000690885838,1.00046048906396,1.))
REPRESENTATION_ITEM('')
);
#382=(
BOUNDED_CURVE()
B_SPLINE_CURVE(2,(#26374,#26375,#26376),.UNSPECIFIED.,.F.,.F.)
B_SPLINE_CURVE_WITH_KNOTS((3,3),(0.,0.118962256406328),.UNSPECIFIED.)
CURVE()
GEOMETRIC_REPRESENTATION_ITEM()
RATIONAL_B_SPLINE_CURVE((1.,1.00046048906152,1.00000690885834))
REPRESENTATION_ITEM('')
);
#383=(
BOUNDED_CURVE()
B_SPLINE_CURVE(2,(#26385,#26386,#26387),.UNSPECIFIED.,.F.,.F.)
B_SPLINE_CURVE_WITH_KNOTS((3,3),(-47.8696729569843,-47.8687190848818),
 .UNSPECIFIED.)
CURVE()
GEOMETRIC_REPRESENTATION_ITEM()
RATIONAL_B_SPLINE_CURVE((15.2054806811781,15.207782406081,15.2100840336132))
REPRESENTATION_ITEM('')
);
#384=(
BOUNDED_CURVE()
B_SPLINE_CURVE(2,(#26390,#26391,#26392),.UNSPECIFIED.,.F.,.F.)
B_SPLINE_CURVE_WITH_KNOTS((3,3),(-2.7739348740092,-2.77298100190679),
 .UNSPECIFIED.)
CURVE()
GEOMETRIC_REPRESENTATION_ITEM()
RATIONAL_B_SPLINE_CURVE((15.2100840336132,15.2077824060811,15.2054806811781))
REPRESENTATION_ITEM('')
);
#385=(
BOUNDED_CURVE()
B_SPLINE_CURVE(2,(#26397,#26398,#26399),.UNSPECIFIED.,.F.,.F.)
B_SPLINE_CURVE_WITH_KNOTS((3,3),(0.111140514111405,0.111966209987666),
 .UNSPECIFIED.)
CURVE()
GEOMETRIC_REPRESENTATION_ITEM()
RATIONAL_B_SPLINE_CURVE((1.00000394455238,1.00000198692881,1.))
REPRESENTATION_ITEM('')
);
#386=(
BOUNDED_CURVE()
B_SPLINE_CURVE(2,(#26404,#26405,#26406),.UNSPECIFIED.,.F.,.F.)
B_SPLINE_CURVE_WITH_KNOTS((3,3),(0.,0.000825695877819724),.UNSPECIFIED.)
CURVE()
GEOMETRIC_REPRESENTATION_ITEM()
RATIONAL_B_SPLINE_CURVE((1.,1.00000198693025,1.00000394455522))
REPRESENTATION_ITEM('')
);
#387=(
BOUNDED_CURVE()
B_SPLINE_CURVE(2,(#26412,#26413,#26414),.UNSPECIFIED.,.F.,.F.)
B_SPLINE_CURVE_WITH_KNOTS((3,3),(0.000899158750380705,0.119861415155793),
 .UNSPECIFIED.)
CURVE()
GEOMETRIC_REPRESENTATION_ITEM()
RATIONAL_B_SPLINE_CURVE((1.00000690885837,1.0004604890632,1.))
REPRESENTATION_ITEM('')
);
#388=(
BOUNDED_CURVE()
B_SPLINE_CURVE(2,(#26421,#26422,#26423),.UNSPECIFIED.,.F.,.F.)
B_SPLINE_CURVE_WITH_KNOTS((3,3),(0.,0.118962256406331),.UNSPECIFIED.)
CURVE()
GEOMETRIC_REPRESENTATION_ITEM()
RATIONAL_B_SPLINE_CURVE((1.,1.00046048906486,1.00000690885839))
REPRESENTATION_ITEM('')
);
#389=(
BOUNDED_CURVE()
B_SPLINE_CURVE(2,(#26432,#26433,#26434),.UNSPECIFIED.,.F.,.F.)
B_SPLINE_CURVE_WITH_KNOTS((3,3),(-47.8696729569845,-47.8687190848821),
 .UNSPECIFIED.)
CURVE()
GEOMETRIC_REPRESENTATION_ITEM()
RATIONAL_B_SPLINE_CURVE((15.2054806811783,15.2077824060812,15.2100840336134))
REPRESENTATION_ITEM('')
);
#390=(
BOUNDED_CURVE()
B_SPLINE_CURVE(2,(#26437,#26438,#26439),.UNSPECIFIED.,.F.,.F.)
B_SPLINE_CURVE_WITH_KNOTS((3,3),(-2.77393487400922,-2.77298100190681),
 .UNSPECIFIED.)
CURVE()
GEOMETRIC_REPRESENTATION_ITEM()
RATIONAL_B_SPLINE_CURVE((15.2100840336133,15.2077824060812,15.2054806811782))
REPRESENTATION_ITEM('')
);
#391=(
BOUNDED_CURVE()
B_SPLINE_CURVE(2,(#26444,#26445,#26446),.UNSPECIFIED.,.F.,.F.)
B_SPLINE_CURVE_WITH_KNOTS((3,3),(0.111140514110649,0.111966209987666),
 .UNSPECIFIED.)
CURVE()
GEOMETRIC_REPRESENTATION_ITEM()
RATIONAL_B_SPLINE_CURVE((1.00000394455082,1.00000198692803,1.))
REPRESENTATION_ITEM('')
);
#392=(
BOUNDED_CURVE()
B_SPLINE_CURVE(2,(#26451,#26452,#26453),.UNSPECIFIED.,.F.,.F.)
B_SPLINE_CURVE_WITH_KNOTS((3,3),(0.,0.000825695875329356),.UNSPECIFIED.)
CURVE()
GEOMETRIC_REPRESENTATION_ITEM()
RATIONAL_B_SPLINE_CURVE((1.,1.00000198692802,1.00000394455079))
REPRESENTATION_ITEM('')
);
#393=(
BOUNDED_CURVE()
B_SPLINE_CURVE(2,(#26459,#26460,#26461),.UNSPECIFIED.,.F.,.F.)
B_SPLINE_CURVE_WITH_KNOTS((3,3),(0.000899158750382631,0.119861415155793),
 .UNSPECIFIED.)
CURVE()
GEOMETRIC_REPRESENTATION_ITEM()
RATIONAL_B_SPLINE_CURVE((1.00000690885839,1.0004604890648,1.))
REPRESENTATION_ITEM('')
);
#394=(
BOUNDED_CURVE()
B_SPLINE_CURVE(2,(#26468,#26469,#26470),.UNSPECIFIED.,.F.,.F.)
B_SPLINE_CURVE_WITH_KNOTS((3,3),(0.,0.118962256406331),.UNSPECIFIED.)
CURVE()
GEOMETRIC_REPRESENTATION_ITEM()
RATIONAL_B_SPLINE_CURVE((1.,1.00046048906397,1.00000690885837))
REPRESENTATION_ITEM('')
);
#395=(
BOUNDED_CURVE()
B_SPLINE_CURVE(2,(#26479,#26480,#26481),.UNSPECIFIED.,.F.,.F.)
B_SPLINE_CURVE_WITH_KNOTS((3,3),(-47.8696729569844,-47.868719084882),
 .UNSPECIFIED.)
CURVE()
GEOMETRIC_REPRESENTATION_ITEM()
RATIONAL_B_SPLINE_CURVE((15.2054806811782,15.2077824060812,15.2100840336133))
REPRESENTATION_ITEM('')
);
#396=(
BOUNDED_CURVE()
B_SPLINE_CURVE(2,(#26484,#26485,#26486),.UNSPECIFIED.,.F.,.F.)
B_SPLINE_CURVE_WITH_KNOTS((3,3),(-2.77393487400938,-2.77298100190697),
 .UNSPECIFIED.)
CURVE()
GEOMETRIC_REPRESENTATION_ITEM()
RATIONAL_B_SPLINE_CURVE((15.2100840336132,15.207782406081,15.205480681178))
REPRESENTATION_ITEM('')
);
#397=(
BOUNDED_CURVE()
B_SPLINE_CURVE(2,(#26491,#26492,#26493),.UNSPECIFIED.,.F.,.F.)
B_SPLINE_CURVE_WITH_KNOTS((3,3),(0.111140514111592,0.111966209987666),
 .UNSPECIFIED.)
CURVE()
GEOMETRIC_REPRESENTATION_ITEM()
RATIONAL_B_SPLINE_CURVE((1.00000394455076,1.000001986928,1.))
REPRESENTATION_ITEM('')
);
#398=(
BOUNDED_CURVE()
B_SPLINE_CURVE(2,(#26498,#26499,#26500),.UNSPECIFIED.,.F.,.F.)
B_SPLINE_CURVE_WITH_KNOTS((3,3),(0.,0.00082569587425766),.UNSPECIFIED.)
CURVE()
GEOMETRIC_REPRESENTATION_ITEM()
RATIONAL_B_SPLINE_CURVE((1.,1.00000198692851,1.00000394455177))
REPRESENTATION_ITEM('')
);
#399=(
BOUNDED_CURVE()
B_SPLINE_CURVE(2,(#26506,#26507,#26508),.UNSPECIFIED.,.F.,.F.)
B_SPLINE_CURVE_WITH_KNOTS((3,3),(0.000899158750379694,0.119861415155793),
 .UNSPECIFIED.)
CURVE()
GEOMETRIC_REPRESENTATION_ITEM()
RATIONAL_B_SPLINE_CURVE((1.00000690885841,1.00046048906573,1.))
REPRESENTATION_ITEM('')
);
#400=(
BOUNDED_CURVE()
B_SPLINE_CURVE(2,(#26515,#26516,#26517),.UNSPECIFIED.,.F.,.F.)
B_SPLINE_CURVE_WITH_KNOTS((3,3),(0.,0.118962256406331),.UNSPECIFIED.)
CURVE()
GEOMETRIC_REPRESENTATION_ITEM()
RATIONAL_B_SPLINE_CURVE((1.,1.00046048906579,1.0000069088584))
REPRESENTATION_ITEM('')
);
#401=(
BOUNDED_CURVE()
B_SPLINE_CURVE(2,(#26526,#26527,#26528),.UNSPECIFIED.,.F.,.F.)
B_SPLINE_CURVE_WITH_KNOTS((3,3),(-47.8696729569842,-47.8687190848818),
 .UNSPECIFIED.)
CURVE()
GEOMETRIC_REPRESENTATION_ITEM()
RATIONAL_B_SPLINE_CURVE((15.205480681178,15.207782406081,15.2100840336131))
REPRESENTATION_ITEM('')
);
#402=(
BOUNDED_CURVE()
B_SPLINE_CURVE(2,(#26531,#26532,#26533),.UNSPECIFIED.,.F.,.F.)
B_SPLINE_CURVE_WITH_KNOTS((3,3),(-2.77393487400937,-2.77298100190696),
 .UNSPECIFIED.)
CURVE()
GEOMETRIC_REPRESENTATION_ITEM()
RATIONAL_B_SPLINE_CURVE((15.2100840336132,15.207782406081,15.205480681178))
REPRESENTATION_ITEM('')
);
#403=(
BOUNDED_CURVE()
B_SPLINE_CURVE(2,(#26538,#26539,#26540),.UNSPECIFIED.,.F.,.F.)
B_SPLINE_CURVE_WITH_KNOTS((3,3),(0.111140514111407,0.111966209987666),
 .UNSPECIFIED.)
CURVE()
GEOMETRIC_REPRESENTATION_ITEM()
RATIONAL_B_SPLINE_CURVE((1.00000394455114,1.00000198692819,1.))
REPRESENTATION_ITEM('')
);
#404=(
BOUNDED_CURVE()
B_SPLINE_CURVE(2,(#26545,#26546,#26547),.UNSPECIFIED.,.F.,.F.)
B_SPLINE_CURVE_WITH_KNOTS((3,3),(0.,0.000825695875568355),.UNSPECIFIED.)
CURVE()
GEOMETRIC_REPRESENTATION_ITEM()
RATIONAL_B_SPLINE_CURVE((1.,1.00000198692854,1.00000394455182))
REPRESENTATION_ITEM('')
);
#405=(
BOUNDED_CURVE()
B_SPLINE_CURVE(2,(#26553,#26554,#26555),.UNSPECIFIED.,.F.,.F.)
B_SPLINE_CURVE_WITH_KNOTS((3,3),(0.000899158750377779,0.119861415155792),
 .UNSPECIFIED.)
CURVE()
GEOMETRIC_REPRESENTATION_ITEM()
RATIONAL_B_SPLINE_CURVE((1.00000690885845,1.00046048906834,1.))
REPRESENTATION_ITEM('')
);
#406=(
BOUNDED_CURVE()
B_SPLINE_CURVE(2,(#26562,#26563,#26564),.UNSPECIFIED.,.F.,.F.)
B_SPLINE_CURVE_WITH_KNOTS((3,3),(0.,0.118962256406334),.UNSPECIFIED.)
CURVE()
GEOMETRIC_REPRESENTATION_ITEM()
RATIONAL_B_SPLINE_CURVE((1.,1.00046048906835,1.00000690885844))
REPRESENTATION_ITEM('')
);
#407=(
BOUNDED_CURVE()
B_SPLINE_CURVE(2,(#26573,#26574,#26575),.UNSPECIFIED.,.F.,.F.)
B_SPLINE_CURVE_WITH_KNOTS((3,3),(-47.8696729569843,-47.8687190848819),
 .UNSPECIFIED.)
CURVE()
GEOMETRIC_REPRESENTATION_ITEM()
RATIONAL_B_SPLINE_CURVE((15.2054806811781,15.2077824060811,15.2100840336133))
REPRESENTATION_ITEM('')
);
#408=(
BOUNDED_CURVE()
B_SPLINE_CURVE(2,(#26578,#26579,#26580),.UNSPECIFIED.,.F.,.F.)
B_SPLINE_CURVE_WITH_KNOTS((3,3),(-2.77393487400929,-2.77298100190688),
 .UNSPECIFIED.)
CURVE()
GEOMETRIC_REPRESENTATION_ITEM()
RATIONAL_B_SPLINE_CURVE((15.2100840336132,15.207782406081,15.205480681178))
REPRESENTATION_ITEM('')
);
#409=(
BOUNDED_CURVE()
B_SPLINE_CURVE(2,(#26586,#26587,#26588),.UNSPECIFIED.,.F.,.F.)
B_SPLINE_CURVE_WITH_KNOTS((3,3),(0.,0.000825695878712508),.UNSPECIFIED.)
CURVE()
GEOMETRIC_REPRESENTATION_ITEM()
RATIONAL_B_SPLINE_CURVE((1.,1.00000198693036,1.00000394455544))
REPRESENTATION_ITEM('')
);
#410=(
BOUNDED_CURVE()
B_SPLINE_CURVE(2,(#26592,#26593,#26594),.UNSPECIFIED.,.F.,.F.)
B_SPLINE_CURVE_WITH_KNOTS((3,3),(0.0008991587503824,0.119861415155793),
 .UNSPECIFIED.)
CURVE()
GEOMETRIC_REPRESENTATION_ITEM()
RATIONAL_B_SPLINE_CURVE((1.0000069088584,1.00046048906496,1.))
REPRESENTATION_ITEM('')
);
#411=(
BOUNDED_CURVE()
B_SPLINE_CURVE(2,(#26596,#26597,#26598),.UNSPECIFIED.,.F.,.F.)
B_SPLINE_CURVE_WITH_KNOTS((3,3),(0.111140514113447,0.111966209987666),
 .UNSPECIFIED.)
CURVE()
GEOMETRIC_REPRESENTATION_ITEM()
RATIONAL_B_SPLINE_CURVE((1.0000039445487,1.00000198692696,1.))
REPRESENTATION_ITEM('')
);
#412=(
BOUNDED_CURVE()
B_SPLINE_CURVE(2,(#26624,#26625,#26626),.UNSPECIFIED.,.F.,.F.)
B_SPLINE_CURVE_WITH_KNOTS((3,3),(0.,0.118962256406329),.UNSPECIFIED.)
CURVE()
GEOMETRIC_REPRESENTATION_ITEM()
RATIONAL_B_SPLINE_CURVE((1.,1.00046048906511,1.00000690885839))
REPRESENTATION_ITEM('')
);
#413=(
BOUNDED_CURVE()
B_SPLINE_CURVE(2,(#26635,#26636,#26637),.UNSPECIFIED.,.F.,.F.)
B_SPLINE_CURVE_WITH_KNOTS((3,3),(-47.8696729569844,-47.868719084882),
 .UNSPECIFIED.)
CURVE()
GEOMETRIC_REPRESENTATION_ITEM()
RATIONAL_B_SPLINE_CURVE((15.2054806811782,15.2077824060812,15.2100840336133))
REPRESENTATION_ITEM('')
);
#414=(
BOUNDED_CURVE()
B_SPLINE_CURVE(2,(#26640,#26641,#26642),.UNSPECIFIED.,.F.,.F.)
B_SPLINE_CURVE_WITH_KNOTS((3,3),(-2.77393487400909,-2.77298100190668),
 .UNSPECIFIED.)
CURVE()
GEOMETRIC_REPRESENTATION_ITEM()
RATIONAL_B_SPLINE_CURVE((15.2100840336134,15.2077824060812,15.2054806811782))
REPRESENTATION_ITEM('')
);
#415=(
BOUNDED_CURVE()
B_SPLINE_CURVE(2,(#26648,#26649,#26650),.UNSPECIFIED.,.F.,.F.)
B_SPLINE_CURVE_WITH_KNOTS((3,3),(0.,0.000825695876243723),.UNSPECIFIED.)
CURVE()
GEOMETRIC_REPRESENTATION_ITEM()
RATIONAL_B_SPLINE_CURVE((1.,1.00000198692885,1.00000394455244))
REPRESENTATION_ITEM('')
);
#416=(
BOUNDED_CURVE()
B_SPLINE_CURVE(2,(#26716,#26717,#26718),.UNSPECIFIED.,.F.,.F.)
B_SPLINE_CURVE_WITH_KNOTS((3,3),(0.111140514108954,0.111966209987666),
 .UNSPECIFIED.)
CURVE()
GEOMETRIC_REPRESENTATION_ITEM()
RATIONAL_B_SPLINE_CURVE((1.00000394455544,1.00000198693036,1.))
REPRESENTATION_ITEM('')
);
#417=FACE_BOUND('',#2507,.T.);
#418=FACE_BOUND('',#2510,.T.);
#419=FACE_BOUND('',#2514,.T.);
#420=FACE_BOUND('',#2518,.T.);
#421=FACE_BOUND('',#2524,.T.);
#422=FACE_BOUND('',#2525,.T.);
#423=FACE_BOUND('',#2526,.T.);
#424=FACE_BOUND('',#2527,.T.);
#425=FACE_BOUND('',#2528,.T.);
#426=FACE_BOUND('',#2556,.T.);
#427=FACE_BOUND('',#2557,.T.);
#428=FACE_BOUND('',#2558,.T.);
#429=FACE_BOUND('',#2612,.T.);
#430=FACE_BOUND('',#2613,.T.);
#431=FACE_BOUND('',#2629,.T.);
#432=FACE_BOUND('',#2632,.T.);
#433=FACE_BOUND('',#2635,.T.);
#434=FACE_BOUND('',#2637,.T.);
#435=FACE_BOUND('',#2644,.T.);
#436=FACE_BOUND('',#2648,.T.);
#437=FACE_BOUND('',#2709,.T.);
#438=FACE_BOUND('',#2710,.T.);
#439=FACE_BOUND('',#2711,.T.);
#440=FACE_BOUND('',#2712,.T.);
#441=FACE_BOUND('',#2713,.T.);
#442=FACE_BOUND('',#2747,.T.);
#443=FACE_BOUND('',#2748,.T.);
#444=FACE_BOUND('',#2749,.T.);
#445=FACE_BOUND('',#2750,.T.);
#446=FACE_BOUND('',#2751,.T.);
#447=FACE_BOUND('',#2760,.T.);
#448=FACE_BOUND('',#2761,.T.);
#449=FACE_BOUND('',#2762,.T.);
#450=FACE_BOUND('',#2765,.T.);
#451=FACE_BOUND('',#2770,.T.);
#452=FACE_BOUND('',#2773,.T.);
#453=FACE_BOUND('',#2818,.T.);
#454=FACE_BOUND('',#2832,.T.);
#455=FACE_BOUND('',#2841,.T.);
#456=FACE_BOUND('',#2844,.T.);
#457=FACE_BOUND('',#2851,.T.);
#458=FACE_BOUND('',#2852,.T.);
#459=FACE_BOUND('',#2853,.T.);
#460=FACE_BOUND('',#2854,.T.);
#461=FACE_BOUND('',#2855,.T.);
#462=FACE_BOUND('',#2856,.T.);
#463=FACE_BOUND('',#2857,.T.);
#464=FACE_BOUND('',#2858,.T.);
#465=FACE_BOUND('',#2871,.T.);
#466=FACE_BOUND('',#2872,.T.);
#467=FACE_BOUND('',#2873,.T.);
#468=FACE_BOUND('',#2874,.T.);
#469=FACE_BOUND('',#2875,.T.);
#470=FACE_BOUND('',#2876,.T.);
#471=FACE_BOUND('',#2877,.T.);
#472=FACE_BOUND('',#2878,.T.);
#473=FACE_BOUND('',#2882,.T.);
#474=FACE_BOUND('',#2886,.T.);
#475=FACE_BOUND('',#2890,.T.);
#476=FACE_BOUND('',#2894,.T.);
#477=FACE_BOUND('',#2898,.T.);
#478=FACE_BOUND('',#2902,.T.);
#479=FACE_BOUND('',#2906,.T.);
#480=FACE_BOUND('',#2926,.T.);
#481=FACE_BOUND('',#2927,.T.);
#482=FACE_BOUND('',#2928,.T.);
#483=FACE_BOUND('',#2931,.T.);
#484=FACE_BOUND('',#2932,.T.);
#485=FACE_BOUND('',#2933,.T.);
#486=FACE_BOUND('',#3042,.T.);
#487=FACE_BOUND('',#3063,.T.);
#488=FACE_BOUND('',#3066,.T.);
#489=FACE_BOUND('',#3069,.T.);
#490=FACE_BOUND('',#3071,.T.);
#491=FACE_BOUND('',#3094,.T.);
#492=FACE_BOUND('',#3097,.T.);
#493=FACE_BOUND('',#3102,.T.);
#494=FACE_BOUND('',#3105,.T.);
#495=FACE_BOUND('',#3108,.T.);
#496=FACE_BOUND('',#3113,.T.);
#497=FACE_BOUND('',#3116,.T.);
#498=FACE_BOUND('',#3118,.T.);
#499=FACE_BOUND('',#3122,.T.);
#500=FACE_BOUND('',#3125,.T.);
#501=FACE_BOUND('',#3128,.T.);
#502=FACE_BOUND('',#3131,.T.);
#503=FACE_BOUND('',#3134,.T.);
#504=FACE_BOUND('',#3138,.T.);
#505=FACE_BOUND('',#3142,.T.);
#506=FACE_BOUND('',#3145,.T.);
#507=FACE_BOUND('',#3150,.T.);
#508=FACE_BOUND('',#3153,.T.);
#509=FACE_BOUND('',#3156,.T.);
#510=FACE_BOUND('',#3163,.T.);
#511=FACE_BOUND('',#3167,.T.);
#512=FACE_BOUND('',#3170,.T.);
#513=FACE_BOUND('',#3172,.T.);
#514=FACE_BOUND('',#3175,.T.);
#515=FACE_BOUND('',#3178,.T.);
#516=FACE_BOUND('',#3194,.T.);
#517=FACE_BOUND('',#3424,.T.);
#518=FACE_BOUND('',#3426,.T.);
#519=FACE_BOUND('',#3427,.T.);
#520=FACE_BOUND('',#3428,.T.);
#521=FACE_BOUND('',#3429,.T.);
#522=FACE_BOUND('',#3430,.T.);
#523=FACE_BOUND('',#3431,.T.);
#524=FACE_BOUND('',#3432,.T.);
#525=FACE_BOUND('',#3433,.T.);
#526=FACE_BOUND('',#3434,.T.);
#527=FACE_BOUND('',#3435,.T.);
#528=FACE_BOUND('',#3436,.T.);
#529=FACE_BOUND('',#3437,.T.);
#530=FACE_BOUND('',#3438,.T.);
#531=FACE_BOUND('',#3439,.T.);
#532=FACE_BOUND('',#3440,.T.);
#533=FACE_BOUND('',#3441,.T.);
#534=FACE_BOUND('',#3442,.T.);
#535=FACE_BOUND('',#3443,.T.);
#536=FACE_BOUND('',#3444,.T.);
#537=FACE_BOUND('',#3445,.T.);
#538=FACE_BOUND('',#3446,.T.);
#539=FACE_BOUND('',#3447,.T.);
#540=FACE_BOUND('',#3448,.T.);
#541=FACE_BOUND('',#3449,.T.);
#542=FACE_BOUND('',#3450,.T.);
#543=FACE_BOUND('',#3451,.T.);
#544=FACE_BOUND('',#3452,.T.);
#545=FACE_BOUND('',#3453,.T.);
#546=FACE_BOUND('',#3454,.T.);
#547=FACE_BOUND('',#3455,.T.);
#548=FACE_BOUND('',#3456,.T.);
#549=FACE_BOUND('',#3457,.T.);
#550=FACE_BOUND('',#3458,.T.);
#551=FACE_BOUND('',#3459,.T.);
#552=FACE_BOUND('',#3460,.T.);
#553=FACE_BOUND('',#3463,.T.);
#554=FACE_BOUND('',#3500,.T.);
#555=FACE_BOUND('',#3515,.T.);
#556=FACE_BOUND('',#3524,.T.);
#557=FACE_BOUND('',#3526,.T.);
#558=PLANE('',#15260);
#559=PLANE('',#15265);
#560=PLANE('',#15274);
#561=PLANE('',#15282);
#562=PLANE('',#15295);
#563=PLANE('',#15320);
#564=PLANE('',#15322);
#565=PLANE('',#15323);
#566=PLANE('',#15325);
#567=PLANE('',#15326);
#568=PLANE('',#15330);
#569=PLANE('',#15339);
#570=PLANE('',#15341);
#571=PLANE('',#15342);
#572=PLANE('',#15344);
#573=PLANE('',#15345);
#574=PLANE('',#15349);
#575=PLANE('',#15358);
#576=PLANE('',#15382);
#577=PLANE('',#15391);
#578=PLANE('',#15393);
#579=PLANE('',#15401);
#580=PLANE('',#15414);
#581=PLANE('',#15422);
#582=PLANE('',#15430);
#583=PLANE('',#15438);
#584=PLANE('',#15473);
#585=PLANE('',#15474);
#586=PLANE('',#15475);
#587=PLANE('',#15476);
#588=PLANE('',#15480);
#589=PLANE('',#15484);
#590=PLANE('',#15488);
#591=PLANE('',#15489);
#592=PLANE('',#15492);
#593=PLANE('',#15493);
#594=PLANE('',#15499);
#595=PLANE('',#15506);
#596=PLANE('',#15519);
#597=PLANE('',#15530);
#598=PLANE('',#15549);
#599=PLANE('',#15567);
#600=PLANE('',#15580);
#601=PLANE('',#15623);
#602=PLANE('',#15642);
#603=PLANE('',#15643);
#604=PLANE('',#15644);
#605=PLANE('',#15669);
#606=PLANE('',#15674);
#607=PLANE('',#15687);
#608=PLANE('',#15695);
#609=PLANE('',#15709);
#610=PLANE('',#15731);
#611=PLANE('',#15734);
#612=PLANE('',#15780);
#613=PLANE('',#15782);
#614=PLANE('',#15783);
#615=PLANE('',#15784);
#616=PLANE('',#15785);
#617=PLANE('',#15786);
#618=PLANE('',#15787);
#619=PLANE('',#15788);
#620=PLANE('',#15789);
#621=PLANE('',#15790);
#622=PLANE('',#15791);
#623=PLANE('',#15794);
#624=PLANE('',#15797);
#625=PLANE('',#15798);
#626=PLANE('',#15800);
#627=PLANE('',#15803);
#628=PLANE('',#15810);
#629=PLANE('',#15812);
#630=PLANE('',#15815);
#631=PLANE('',#15817);
#632=PLANE('',#15820);
#633=PLANE('',#15824);
#634=PLANE('',#15830);
#635=PLANE('',#15841);
#636=PLANE('',#15843);
#637=PLANE('',#15845);
#638=PLANE('',#15846);
#639=PLANE('',#15847);
#640=PLANE('',#15852);
#641=PLANE('',#15853);
#642=PLANE('',#15854);
#643=PLANE('',#15855);
#644=PLANE('',#15856);
#645=PLANE('',#15869);
#646=PLANE('',#15874);
#647=PLANE('',#15879);
#648=PLANE('',#15884);
#649=PLANE('',#15889);
#650=PLANE('',#15894);
#651=PLANE('',#15899);
#652=PLANE('',#15902);
#653=PLANE('',#15905);
#654=PLANE('',#15906);
#655=PLANE('',#15909);
#656=PLANE('',#15912);
#657=PLANE('',#15913);
#658=PLANE('',#15916);
#659=PLANE('',#15919);
#660=PLANE('',#15920);
#661=PLANE('',#15923);
#662=PLANE('',#15926);
#663=PLANE('',#15927);
#664=PLANE('',#15945);
#665=PLANE('',#15949);
#666=PLANE('',#15951);
#667=PLANE('',#15952);
#668=PLANE('',#15956);
#669=PLANE('',#15957);
#670=PLANE('',#15958);
#671=PLANE('',#15959);
#672=PLANE('',#15960);
#673=PLANE('',#15964);
#674=PLANE('',#15965);
#675=PLANE('',#15966);
#676=PLANE('',#15967);
#677=PLANE('',#15968);
#678=PLANE('',#15972);
#679=PLANE('',#15973);
#680=PLANE('',#15974);
#681=PLANE('',#15975);
#682=PLANE('',#15976);
#683=PLANE('',#15980);
#684=PLANE('',#15981);
#685=PLANE('',#15982);
#686=PLANE('',#15983);
#687=PLANE('',#15984);
#688=PLANE('',#15985);
#689=PLANE('',#15989);
#690=PLANE('',#16016);
#691=PLANE('',#16017);
#692=PLANE('',#16020);
#693=PLANE('',#16021);
#694=PLANE('',#16022);
#695=PLANE('',#16023);
#696=PLANE('',#16024);
#697=PLANE('',#16027);
#698=PLANE('',#16028);
#699=PLANE('',#16029);
#700=PLANE('',#16030);
#701=PLANE('',#16031);
#702=PLANE('',#16032);
#703=PLANE('',#16033);
#704=PLANE('',#16034);
#705=PLANE('',#16035);
#706=PLANE('',#16036);
#707=PLANE('',#16037);
#708=PLANE('',#16038);
#709=PLANE('',#16039);
#710=PLANE('',#16040);
#711=PLANE('',#16041);
#712=PLANE('',#16042);
#713=PLANE('',#16043);
#714=PLANE('',#16044);
#715=PLANE('',#16045);
#716=PLANE('',#16046);
#717=PLANE('',#16047);
#718=PLANE('',#16048);
#719=PLANE('',#16049);
#720=PLANE('',#16050);
#721=PLANE('',#16051);
#722=PLANE('',#16052);
#723=PLANE('',#16053);
#724=PLANE('',#16054);
#725=PLANE('',#16055);
#726=PLANE('',#16058);
#727=PLANE('',#16059);
#728=PLANE('',#16060);
#729=PLANE('',#16061);
#730=PLANE('',#16062);
#731=PLANE('',#16065);
#732=PLANE('',#16066);
#733=PLANE('',#16067);
#734=PLANE('',#16068);
#735=PLANE('',#16069);
#736=PLANE('',#16072);
#737=PLANE('',#16073);
#738=PLANE('',#16074);
#739=PLANE('',#16075);
#740=PLANE('',#16076);
#741=PLANE('',#16079);
#742=PLANE('',#16080);
#743=PLANE('',#16081);
#744=PLANE('',#16082);
#745=PLANE('',#16083);
#746=PLANE('',#16086);
#747=PLANE('',#16087);
#748=PLANE('',#16090);
#749=PLANE('',#16091);
#750=PLANE('',#16092);
#751=PLANE('',#16093);
#752=PLANE('',#16096);
#753=PLANE('',#16097);
#754=PLANE('',#16105);
#755=PLANE('',#16116);
#756=PLANE('',#16117);
#757=PLANE('',#16119);
#758=PLANE('',#16120);
#759=PLANE('',#16121);
#760=PLANE('',#16123);
#761=PLANE('',#16124);
#762=PLANE('',#16129);
#763=PLANE('',#16135);
#764=PLANE('',#16137);
#765=PLANE('',#16141);
#766=PLANE('',#16145);
#767=PLANE('',#16151);
#768=PLANE('',#16153);
#769=PLANE('',#16154);
#770=PLANE('',#16155);
#771=PLANE('',#16156);
#772=PLANE('',#16157);
#773=PLANE('',#16158);
#774=PLANE('',#16159);
#775=PLANE('',#16160);
#776=PLANE('',#16161);
#777=PLANE('',#16162);
#778=PLANE('',#16163);
#779=PLANE('',#16164);
#780=PLANE('',#16165);
#781=PLANE('',#16166);
#782=PLANE('',#16167);
#783=PLANE('',#16168);
#784=PLANE('',#16169);
#785=PLANE('',#16170);
#786=PLANE('',#16175);
#787=PLANE('',#16179);
#788=PLANE('',#16187);
#789=PLANE('',#16191);
#790=PLANE('',#16195);
#791=PLANE('',#16203);
#792=PLANE('',#16208);
#793=PLANE('',#16210);
#794=PLANE('',#16217);
#795=PLANE('',#16221);
#796=PLANE('',#16225);
#797=PLANE('',#16228);
#798=PLANE('',#16234);
#799=PLANE('',#16242);
#800=PLANE('',#16248);
#801=PLANE('',#16251);
#802=PLANE('',#16260);
#803=PLANE('',#16266);
#804=PLANE('',#16271);
#805=PLANE('',#16283);
#806=PLANE('',#16289);
#807=PLANE('',#16293);
#808=PLANE('',#16303);
#809=PLANE('',#16309);
#810=PLANE('',#16352);
#811=PLANE('',#16428);
#812=PLANE('',#16433);
#813=PLANE('',#16434);
#814=PLANE('',#16436);
#815=PLANE('',#16437);
#816=PLANE('',#16439);
#817=PLANE('',#16440);
#818=PLANE('',#16442);
#819=PLANE('',#16443);
#820=PLANE('',#16445);
#821=PLANE('',#16446);
#822=PLANE('',#16448);
#823=PLANE('',#16449);
#824=PLANE('',#16451);
#825=PLANE('',#16452);
#826=PLANE('',#16454);
#827=PLANE('',#16455);
#828=PLANE('',#16457);
#829=PLANE('',#16458);
#830=PLANE('',#16460);
#831=PLANE('',#16461);
#832=PLANE('',#16463);
#833=PLANE('',#16464);
#834=PLANE('',#16466);
#835=PLANE('',#16467);
#836=PLANE('',#16469);
#837=PLANE('',#16470);
#838=PLANE('',#16472);
#839=PLANE('',#16473);
#840=PLANE('',#16475);
#841=PLANE('',#16476);
#842=PLANE('',#16478);
#843=PLANE('',#16479);
#844=PLANE('',#16481);
#845=PLANE('',#16482);
#846=PLANE('',#16484);
#847=PLANE('',#16485);
#848=PLANE('',#16487);
#849=PLANE('',#16488);
#850=PLANE('',#16490);
#851=PLANE('',#16491);
#852=PLANE('',#16493);
#853=PLANE('',#16494);
#854=PLANE('',#16496);
#855=PLANE('',#16497);
#856=PLANE('',#16499);
#857=PLANE('',#16500);
#858=PLANE('',#16502);
#859=PLANE('',#16503);
#860=PLANE('',#16505);
#861=PLANE('',#16506);
#862=PLANE('',#16508);
#863=PLANE('',#16509);
#864=PLANE('',#16511);
#865=PLANE('',#16512);
#866=PLANE('',#16514);
#867=PLANE('',#16515);
#868=PLANE('',#16517);
#869=PLANE('',#16518);
#870=PLANE('',#16520);
#871=PLANE('',#16521);
#872=PLANE('',#16523);
#873=PLANE('',#16524);
#874=PLANE('',#16526);
#875=PLANE('',#16527);
#876=PLANE('',#16529);
#877=PLANE('',#16530);
#878=PLANE('',#16532);
#879=PLANE('',#16533);
#880=PLANE('',#16535);
#881=PLANE('',#16536);
#882=PLANE('',#16539);
#883=PLANE('',#16540);
#884=PLANE('',#16543);
#885=PLANE('',#16544);
#886=PLANE('',#16546);
#887=PLANE('',#16547);
#888=PLANE('',#16549);
#889=PLANE('',#16550);
#890=PLANE('',#16552);
#891=PLANE('',#16553);
#892=PLANE('',#16555);
#893=PLANE('',#16556);
#894=PLANE('',#16558);
#895=PLANE('',#16559);
#896=PLANE('',#16561);
#897=PLANE('',#16562);
#898=PLANE('',#16564);
#899=PLANE('',#16565);
#900=PLANE('',#16567);
#901=PLANE('',#16568);
#902=PLANE('',#16570);
#903=PLANE('',#16571);
#904=PLANE('',#16573);
#905=PLANE('',#16574);
#906=PLANE('',#16576);
#907=PLANE('',#16577);
#908=PLANE('',#16579);
#909=PLANE('',#16580);
#910=PLANE('',#16582);
#911=PLANE('',#16583);
#912=PLANE('',#16585);
#913=PLANE('',#16586);
#914=PLANE('',#16588);
#915=PLANE('',#16589);
#916=PLANE('',#16591);
#917=PLANE('',#16592);
#918=PLANE('',#16594);
#919=PLANE('',#16595);
#920=PLANE('',#16597);
#921=PLANE('',#16598);
#922=PLANE('',#16600);
#923=PLANE('',#16601);
#924=PLANE('',#16603);
#925=PLANE('',#16604);
#926=PLANE('',#16606);
#927=PLANE('',#16607);
#928=PLANE('',#16609);
#929=PLANE('',#16610);
#930=PLANE('',#16612);
#931=PLANE('',#16613);
#932=PLANE('',#16615);
#933=PLANE('',#16616);
#934=PLANE('',#16618);
#935=PLANE('',#16619);
#936=PLANE('',#16621);
#937=PLANE('',#16622);
#938=PLANE('',#16624);
#939=PLANE('',#16625);
#940=PLANE('',#16627);
#941=PLANE('',#16628);
#942=PLANE('',#16630);
#943=PLANE('',#16631);
#944=PLANE('',#16633);
#945=PLANE('',#16634);
#946=PLANE('',#16636);
#947=PLANE('',#16637);
#948=PLANE('',#16639);
#949=PLANE('',#16640);
#950=PLANE('',#16642);
#951=PLANE('',#16643);
#952=PLANE('',#16645);
#953=PLANE('',#16646);
#954=PLANE('',#16648);
#955=PLANE('',#16649);
#956=PLANE('',#16651);
#957=PLANE('',#16652);
#958=PLANE('',#16653);
#959=PLANE('',#16654);
#960=PLANE('',#16655);
#961=PLANE('',#16656);
#962=PLANE('',#16657);
#963=PLANE('',#16658);
#964=PLANE('',#16663);
#965=PLANE('',#16669);
#966=PLANE('',#16688);
#967=PLANE('',#16689);
#968=PLANE('',#16690);
#969=PLANE('',#16691);
#970=PLANE('',#16692);
#971=PLANE('',#16693);
#972=PLANE('',#16694);
#973=PLANE('',#16695);
#974=PLANE('',#16696);
#975=PLANE('',#16697);
#976=PLANE('',#16698);
#977=PLANE('',#16699);
#978=PLANE('',#16700);
#979=PLANE('',#16701);
#980=PLANE('',#16702);
#981=PLANE('',#16703);
#982=PLANE('',#16704);
#983=PLANE('',#16705);
#984=PLANE('',#16706);
#985=PLANE('',#16707);
#986=PLANE('',#16708);
#987=PLANE('',#16709);
#988=PLANE('',#16710);
#989=PLANE('',#16711);
#990=PLANE('',#16712);
#991=PLANE('',#16713);
#992=PLANE('',#16714);
#993=PLANE('',#16715);
#994=PLANE('',#16716);
#995=PLANE('',#16717);
#996=PLANE('',#16718);
#997=PLANE('',#16719);
#998=PLANE('',#16724);
#999=PLANE('',#16727);
#1000=PLANE('',#16728);
#1001=PLANE('',#16729);
#1002=PLANE('',#16730);
#1003=PLANE('',#16731);
#1004=PLANE('',#16732);
#1005=PLANE('',#16733);
#1006=PLANE('',#16734);
#1007=PLANE('',#16736);
#1008=PLANE('',#16740);
#1009=B_SPLINE_CURVE_WITH_KNOTS('',3,(#20904,#20905,#20906,#20907,#20908,
#20909,#20910,#20911,#20912,#20913),.UNSPECIFIED.,.F.,.F.,(4,2,2,2,4),(3.93196561503714,
3.98793494995107,4.45544073881652,4.92294652768197,4.9789158625959),
 .UNSPECIFIED.);
#1010=B_SPLINE_CURVE_WITH_KNOTS('',3,(#20956,#20957,#20958,#20959,#20960,
#20961,#20962,#20963,#20964,#20965),.UNSPECIFIED.,.F.,.F.,(4,2,2,2,4),(3.93196561503714,
3.98793494995108,4.45544073881652,4.92294652768197,4.97891586259591),
 .UNSPECIFIED.);
#1011=B_SPLINE_CURVE_WITH_KNOTS('',3,(#20998,#20999,#21000,#21001,#21002),
 .UNSPECIFIED.,.F.,.F.,(4,1,4),(4.72327004821084,5.43406096940559,5.4438775737049),
 .UNSPECIFIED.);
#1012=B_SPLINE_CURVE_WITH_KNOTS('',3,(#21005,#21006,#21007,#21008,#21009,
#21010,#21011,#21012,#21013),.UNSPECIFIED.,.F.,.F.,(4,1,1,1,1,1,4),(5.4438775737049,
6.14485189097757,6.85564281254955,7.56643373412153,8.27722465569351,8.98801557726548,
9.69880649883746),.UNSPECIFIED.);
#1013=B_SPLINE_CURVE_WITH_KNOTS('',3,(#21075,#21076,#21077,#21078,#21079,
#21080,#21081,#21082),.UNSPECIFIED.,.F.,.F.,(4,2,2,4),(0.909514729117648,
0.949358494570548,1.0210248366573,1.05494162626089),.UNSPECIFIED.);
#1014=B_SPLINE_CURVE_WITH_KNOTS('',3,(#21086,#21087,#21088,#21089),
 .UNSPECIFIED.,.F.,.F.,(4,4),(-0.0999299837778113,0.),.UNSPECIFIED.);
#1015=B_SPLINE_CURVE_WITH_KNOTS('',3,(#21118,#21119,#21120,#21121,#21122,
#21123,#21124,#21125,#21126,#21127),.UNSPECIFIED.,.F.,.F.,(4,2,2,2,4),(2.62788407869953,
2.67944373713314,2.73012587368336,2.74303185768817,2.7532959630073),
 .UNSPECIFIED.);
#1016=B_SPLINE_CURVE_WITH_KNOTS('',3,(#21137,#21138,#21139,#21140,#21141,
#21142,#21143,#21144,#21145,#21146),.UNSPECIFIED.,.F.,.F.,(4,2,2,2,4),(1.79948460602208,
1.8527312039325,2.06373263634258,2.27473406875267,2.69673693357283),
 .UNSPECIFIED.);
#1017=B_SPLINE_CURVE_WITH_KNOTS('',3,(#21150,#21151,#21152,#21153,#21154,
#21155,#21156,#21157,#21158,#21159),.UNSPECIFIED.,.F.,.F.,(4,2,2,2,4),(4.15220051801173,
4.5742033828319,4.78520481524198,4.99620624765207,5.04945284556248),
 .UNSPECIFIED.);
#1018=B_SPLINE_CURVE_WITH_KNOTS('',3,(#21174,#21175,#21176,#21177,#21178,
#21179,#21180,#21181,#21182,#21183),.UNSPECIFIED.,.F.,.F.,(4,2,2,2,4),(0.917765321002435,
0.928029426321564,0.940935410326375,0.991617546876601,1.04317720531021),
 .UNSPECIFIED.);
#1019=B_SPLINE_CURVE_WITH_KNOTS('',3,(#21189,#21190,#21191,#21192,#21193,
#21194,#21195,#21196),.UNSPECIFIED.,.F.,.F.,(4,2,2,4),(0.423927454431935,
0.457844244035524,0.529510586122272,0.569354351575173),.UNSPECIFIED.);
#1020=B_SPLINE_CURVE_WITH_KNOTS('',3,(#21201,#21202,#21203,#21204),
 .UNSPECIFIED.,.F.,.F.,(4,4),(-0.0999299524181728,0.),.UNSPECIFIED.);
#1021=B_SPLINE_CURVE_WITH_KNOTS('',3,(#21213,#21214,#21215,#21216,#21217,
#21218,#21219,#21220),.UNSPECIFIED.,.F.,.F.,(4,2,2,4),(0.444478348171076,
0.457897885991393,0.533188282866212,0.608478679741031),.UNSPECIFIED.);
#1022=B_SPLINE_CURVE_WITH_KNOTS('',3,(#21227,#21228,#21229,#21230,#21231,
#21232,#21233,#21234),.UNSPECIFIED.,.F.,.F.,(4,2,2,4),(0.608478679741031,
0.68376907661585,0.759059473490669,0.772479011310987),.UNSPECIFIED.);
#1023=B_SPLINE_CURVE_WITH_KNOTS('',3,(#21236,#21237,#21238,#21239,#21240,
#21241,#21242,#21243),.UNSPECIFIED.,.F.,.F.,(4,2,2,4),(1.27628724021533,
1.34251720334849,1.43059045082634,1.8254794159769),.UNSPECIFIED.);
#1024=B_SPLINE_CURVE_WITH_KNOTS('',3,(#21246,#21247,#21248,#21249,#21250,
#21251,#21252,#21253),.UNSPECIFIED.,.F.,.F.,(4,2,2,4),(0.537818085774576,
0.932707050925141,1.02078029840299,1.08701026153615),.UNSPECIFIED.);
#1025=B_SPLINE_CURVE_WITH_KNOTS('',3,(#21256,#21257,#21258,#21259,#21260,
#21261,#21262,#21263),.UNSPECIFIED.,.F.,.F.,(4,2,2,4),(1.27628724021533,
1.34251720334849,1.43059045082634,1.8254794159769),.UNSPECIFIED.);
#1026=B_SPLINE_CURVE_WITH_KNOTS('',3,(#21266,#21267,#21268,#21269,#21270,
#21271,#21272,#21273),.UNSPECIFIED.,.F.,.F.,(4,2,2,4),(0.537818085774576,
0.932707050925141,1.02078029840299,1.08701026153615),.UNSPECIFIED.);
#1027=B_SPLINE_CURVE_WITH_KNOTS('',3,(#21276,#21277,#21278,#21279,#21280,
#21281,#21282,#21283),.UNSPECIFIED.,.F.,.F.,(4,2,2,4),(0.909514729117652,
0.949358494570554,1.0210248366573,1.05494162626089),.UNSPECIFIED.);
#1028=B_SPLINE_CURVE_WITH_KNOTS('',3,(#21287,#21288,#21289,#21290),
 .UNSPECIFIED.,.F.,.F.,(4,4),(-0.099929983777859,0.),.UNSPECIFIED.);
#1029=B_SPLINE_CURVE_WITH_KNOTS('',3,(#21313,#21314,#21315,#21316,#21317,
#21318,#21319,#21320,#21321,#21322),.UNSPECIFIED.,.F.,.F.,(4,2,2,2,4),(2.62788407869953,
2.67944373713314,2.73012587368336,2.74303185768817,2.7532959630073),
 .UNSPECIFIED.);
#1030=B_SPLINE_CURVE_WITH_KNOTS('',3,(#21332,#21333,#21334,#21335,#21336,
#21337,#21338,#21339,#21340,#21341),.UNSPECIFIED.,.F.,.F.,(4,2,2,2,4),(1.79948460602208,
1.8527312039325,2.06373263634258,2.27473406875267,2.69673693357283),
 .UNSPECIFIED.);
#1031=B_SPLINE_CURVE_WITH_KNOTS('',3,(#21345,#21346,#21347,#21348,#21349,
#21350,#21351,#21352,#21353,#21354),.UNSPECIFIED.,.F.,.F.,(4,2,2,2,4),(4.15220051801173,
4.5742033828319,4.78520481524198,4.99620624765207,5.04945284556248),
 .UNSPECIFIED.);
#1032=B_SPLINE_CURVE_WITH_KNOTS('',3,(#21369,#21370,#21371,#21372,#21373,
#21374,#21375,#21376,#21377,#21378),.UNSPECIFIED.,.F.,.F.,(4,2,2,2,4),(0.917765321002435,
0.928029426321564,0.940935410326375,0.991617546876601,1.04317720531021),
 .UNSPECIFIED.);
#1033=B_SPLINE_CURVE_WITH_KNOTS('',3,(#21384,#21385,#21386,#21387,#21388,
#21389,#21390,#21391),.UNSPECIFIED.,.F.,.F.,(4,2,2,4),(0.42392745443194,
0.457844244035527,0.529510586122276,0.569354351575178),.UNSPECIFIED.);
#1034=B_SPLINE_CURVE_WITH_KNOTS('',3,(#21392,#21393,#21394,#21395),
 .UNSPECIFIED.,.F.,.F.,(4,4),(-0.0999299524180764,0.),.UNSPECIFIED.);
#1035=B_SPLINE_CURVE_WITH_KNOTS('',3,(#21402,#21403,#21404,#21405,#21406,
#21407,#21408,#21409),.UNSPECIFIED.,.F.,.F.,(4,2,2,4),(0.444478348171076,
0.457897885991393,0.533188282866212,0.608478679741031),.UNSPECIFIED.);
#1036=B_SPLINE_CURVE_WITH_KNOTS('',3,(#21416,#21417,#21418,#21419,#21420,
#21421,#21422,#21423),.UNSPECIFIED.,.F.,.F.,(4,2,2,4),(0.608478679741031,
0.68376907661585,0.759059473490669,0.772479011310987),.UNSPECIFIED.);
#1037=B_SPLINE_CURVE_WITH_KNOTS('',3,(#21425,#21426,#21427,#21428,#21429,
#21430,#21431,#21432),.UNSPECIFIED.,.F.,.F.,(4,2,2,4),(1.27628724021533,
1.34251720334849,1.43059045082634,1.8254794159769),.UNSPECIFIED.);
#1038=B_SPLINE_CURVE_WITH_KNOTS('',3,(#21435,#21436,#21437,#21438,#21439,
#21440,#21441,#21442),.UNSPECIFIED.,.F.,.F.,(4,2,2,4),(0.537818085774576,
0.932707050925141,1.02078029840299,1.08701026153615),.UNSPECIFIED.);
#1039=B_SPLINE_CURVE_WITH_KNOTS('',3,(#21445,#21446,#21447,#21448,#21449,
#21450,#21451,#21452),.UNSPECIFIED.,.F.,.F.,(4,2,2,4),(1.27628724021533,
1.34251720334849,1.43059045082634,1.8254794159769),.UNSPECIFIED.);
#1040=B_SPLINE_CURVE_WITH_KNOTS('',3,(#21455,#21456,#21457,#21458,#21459,
#21460,#21461,#21462),.UNSPECIFIED.,.F.,.F.,(4,2,2,4),(0.537818085774576,
0.932707050925141,1.02078029840299,1.08701026153615),.UNSPECIFIED.);
#1041=B_SPLINE_CURVE_WITH_KNOTS('',3,(#21491,#21492,#21493,#21494,#21495,
#21496,#21497,#21498,#21499,#21500,#21501,#21502,#21503,#21504),
 .UNSPECIFIED.,.F.,.F.,(4,2,2,2,2,2,4),(-0.0007960460749726,0.,0.0734612670102269,
0.144831741121295,0.230214082122091,0.299049896049864,0.361337990313849),
 .UNSPECIFIED.);
#1042=B_SPLINE_CURVE_WITH_KNOTS('',3,(#21505,#21506,#21507,#21508,#21509,
#21510,#21511,#21512,#21513,#21514,#21515,#21516,#21517,#21518),
 .UNSPECIFIED.,.F.,.F.,(4,2,2,2,2,2,4),(-0.723464285927595,-0.722647521542398,
-0.649394023974264,-0.578539147977434,-0.492689132311904,-0.42364974758642,
-0.361323760770171),.UNSPECIFIED.);
#1043=B_SPLINE_CURVE_WITH_KNOTS('',3,(#21528,#21529,#21530,#21531,#21532,
#21533,#21534,#21535,#21536,#21537,#21538,#21539,#21540,#21541),
 .UNSPECIFIED.,.F.,.F.,(4,2,2,2,2,2,4),(-0.361281373349619,-0.299845297677646,
-0.234790847494551,-0.156277186792366,-0.0770809532846638,0.,0.000773217160646022),
 .UNSPECIFIED.);
#1044=B_SPLINE_CURVE_WITH_KNOTS('',3,(#21544,#21545,#21546,#21547,#21548,
#21549,#21550,#21551,#21552,#21553,#21554,#21555,#21556,#21557),
 .UNSPECIFIED.,.F.,.F.,(4,2,2,2,2,2,4),(-0.723464285923361,-0.722647521538168,
-0.649394023970219,-0.578539147973825,-0.492689132308839,-0.423649747583786,
-0.361323760767944),.UNSPECIFIED.);
#1045=B_SPLINE_CURVE_WITH_KNOTS('',3,(#21692,#21693,#21694,#21695,#21696,
#21697,#21698,#21699,#21700,#21701,#21702,#21703,#21704,#21705,#21706,#21707,
#21708,#21709,#21710,#21711,#21712,#21713,#21714,#21715,#21716),
 .UNSPECIFIED.,.F.,.F.,(4,1,1,1,1,1,1,1,1,1,1,1,1,1,1,1,1,1,1,1,2,4),(0.,
0.0461389911948815,0.0922779823897629,0.115347477987204,0.138416973584644,
0.184555964779526,0.196090712578246,0.207625460376967,0.230694955974407,
0.253764451571848,0.276833947169289,0.29990344276673,0.32297293836417,0.346042433961611,
0.369111929559052,0.392181425156492,0.415250920753933,0.438320416351374,
0.449855164150094,0.455622538049454,0.461389911948815,0.46172446147336),
 .UNSPECIFIED.);
#1046=B_SPLINE_CURVE_WITH_KNOTS('',3,(#21718,#21719,#21720,#21721,#21722,
#21723,#21724,#21725,#21726,#21727),.UNSPECIFIED.,.F.,.F.,(4,1,1,1,1,1,
1,4),(5.2903133410746,5.58533904887944,5.88036475668429,6.17539046448912,
6.47041617229397,6.76544188009881,7.06046758790365,7.35549329570849),
 .UNSPECIFIED.);
#1047=B_SPLINE_CURVE_WITH_KNOTS('',3,(#21729,#21730,#21731,#21732,#21733,
#21734,#21735),.UNSPECIFIED.,.F.,.F.,(4,1,1,1,4),(-4.1253064325321E-6,0.0329961931811326,
0.131997148643828,0.263998422594088,0.462000333519479),.UNSPECIFIED.);
#1048=B_SPLINE_CURVE_WITH_KNOTS('',3,(#21736,#21737,#21738,#21739,#21740,
#21741,#21742,#21743,#21744,#21745,#21746,#21747,#21748,#21749,#21750,#21751,
#21752,#21753,#21754,#21755,#21756,#21757,#21758,#21759,#21760,#21761,#21762,
#21763,#21764,#21765,#21766,#21767,#21768,#21769,#21770,#21771,#21772,#21773,
#21774,#21775,#21776,#21777,#21778,#21779,#21780,#21781,#21782,#21783,#21784,
#21785,#21786,#21787,#21788,#21789,#21790,#21791,#21792,#21793,#21794,#21795,
#21796,#21797,#21798,#21799,#21800,#21801,#21802,#21803,#21804,#21805,#21806,
#21807,#21808,#21809,#21810,#21811,#21812,#21813,#21814,#21815,#21816,#21817,
#21818,#21819,#21820,#21821,#21822,#21823,#21824,#21825,#21826,#21827,#21828,
#21829,#21830,#21831,#21832,#21833,#21834,#21835,#21836,#21837,#21838,#21839,
#21840,#21841,#21842,#21843,#21844,#21845,#21846,#21847,#21848,#21849,#21850,
#21851,#21852,#21853,#21854,#21855,#21856,#21857,#21858,#21859,#21860,#21861,
#21862,#21863,#21864,#21865,#21866,#21867,#21868,#21869,#21870,#21871,#21872,
#21873,#21874,#21875,#21876,#21877,#21878,#21879,#21880,#21881,#21882,#21883,
#21884,#21885,#21886,#21887,#21888,#21889),.UNSPECIFIED.,.F.,.F.,(4,3,3,
3,3,3,3,3,3,3,3,3,3,3,3,3,3,3,3,3,3,3,3,3,3,3,3,3,3,3,3,3,3,3,3,3,3,3,3,
3,3,3,3,3,3,3,3,3,3,3,3,4),(-9.23633566839803,-9.12960054610899,-9.02995313475932,
-8.98820092273608,-8.94767164911647,-8.85551547280586,-8.76973813956101,
-8.76335929649525,-8.67204037852948,-8.58170123880419,-8.50986230805487,
-8.41197083977331,-8.31595106965646,-8.27742304064402,-8.18141772850045,
-8.08522998019979,-8.07506594002406,-7.96624383986804,-7.85665330525787,
-7.74811076545733,-7.64783984054416,-7.56639692453424,-7.46050702505756,
-7.35408928718672,-7.24751062386446,-7.21105298394138,-7.11797817184964,
-7.02480289993274,-6.98739369316414,-6.87981578778465,-6.85563657893624,
-6.75528006343046,-6.64913220023725,-6.54164653415872,-6.43390512945243,
-6.37349276133023,-6.27658287658477,-6.1795448081392,-6.14462846979886,
-6.04725880022175,-5.9475667529657,-5.93469080516676,-5.83694309104053,
-5.73794849627641,-5.67251567403569,-5.57655253596878,-5.48609949444031,
-5.43374272495868,-5.34284104121183,-5.3056567205391,-5.19777701987056,
-5.18574149361684),.UNSPECIFIED.);
#1049=B_SPLINE_CURVE_WITH_KNOTS('',3,(#21892,#21893,#21894,#21895,#21896,
#21897),.UNSPECIFIED.,.F.,.F.,(4,1,1,4),(0.,0.263843142766397,0.395764714149595,
0.461725499841195),.UNSPECIFIED.);
#1050=B_SPLINE_CURVE_WITH_KNOTS('',3,(#21899,#21900,#21901,#21902,#21903,
#21904,#21905,#21906,#21907,#21908),.UNSPECIFIED.,.F.,.F.,(4,1,1,1,1,1,
1,4),(5.29031334107461,5.58533904887945,5.88036475668429,6.17539046448913,
6.47041617229397,6.76544188009881,7.06046758790365,7.35549329570849),
 .UNSPECIFIED.);
#1051=B_SPLINE_CURVE_WITH_KNOTS('',3,(#21910,#21911,#21912,#21913,#21914,
#21915),.UNSPECIFIED.,.F.,.F.,(4,1,1,4),(-3.57706725334641E-6,0.0659639823856703,
0.197899101291517,0.461769339103211),.UNSPECIFIED.);
#1052=B_SPLINE_CURVE_WITH_KNOTS('',3,(#21916,#21917,#21918,#21919,#21920,
#21921,#21922,#21923,#21924,#21925,#21926,#21927,#21928,#21929,#21930,#21931,
#21932,#21933,#21934,#21935,#21936,#21937,#21938,#21939,#21940,#21941,#21942,
#21943,#21944,#21945,#21946,#21947,#21948,#21949,#21950,#21951,#21952,#21953,
#21954,#21955,#21956,#21957,#21958,#21959,#21960,#21961,#21962,#21963,#21964,
#21965,#21966,#21967,#21968,#21969,#21970,#21971,#21972,#21973,#21974,#21975,
#21976,#21977,#21978,#21979,#21980,#21981,#21982,#21983,#21984,#21985,#21986,
#21987,#21988,#21989,#21990,#21991,#21992,#21993,#21994,#21995,#21996,#21997,
#21998,#21999,#22000,#22001,#22002,#22003,#22004,#22005,#22006,#22007,#22008,
#22009,#22010,#22011,#22012,#22013,#22014,#22015,#22016,#22017,#22018,#22019,
#22020,#22021,#22022,#22023,#22024,#22025,#22026,#22027,#22028,#22029,#22030,
#22031,#22032,#22033,#22034,#22035,#22036,#22037,#22038,#22039,#22040,#22041,
#22042,#22043,#22044,#22045,#22046,#22047,#22048,#22049,#22050,#22051,#22052,
#22053,#22054,#22055,#22056,#22057,#22058,#22059,#22060,#22061,#22062,#22063,
#22064,#22065,#22066),.UNSPECIFIED.,.F.,.F.,(4,3,3,3,3,3,3,3,3,3,3,3,3,
3,3,3,3,3,3,3,3,3,3,3,3,3,3,3,3,3,3,3,3,3,3,3,3,3,3,3,3,3,3,3,3,3,3,3,3,
3,4),(-9.23633566861216,-9.12960054616757,-9.0301001347754,-8.98819964439314,
-8.9476716491939,-8.85551547287179,-8.77004832787379,-8.76335929654967,
-8.67183742403758,-8.58130233357639,-8.50986230801197,-8.41188984789292,
-8.31575746142269,-8.277426795238,-8.17624636762553,-8.07506594001306,-7.96541085300417,
-7.85497781952315,-7.74563908368099,-7.64783984052849,-7.56643652217298,
-7.46139284189079,-7.35584564549624,-7.25012317373638,-7.21105298394139,
-7.1181354465781,-7.02511356178625,-6.98739369309937,-6.88169773695743,
-6.85571344061752,-6.75528006328435,-6.64904197167172,-6.54161818053077,
-6.43368025611171,-6.37349276120329,-6.27597952064751,-6.17860698749197,
-6.14486393337072,-6.04674431800307,-5.94656644708164,-5.93469080503813,
-5.83307322116587,-5.7296525497896,-5.67251567404192,-5.56269437350081,
-5.48609949447997,-5.43365613366603,-5.33247743921033,-5.30565672055846,
-5.20312542921902,-5.18574149383096),.UNSPECIFIED.);
#1053=B_SPLINE_CURVE_WITH_KNOTS('',3,(#22096,#22097,#22098,#22099,#22100,
#22101,#22102,#22103,#22104,#22105,#22106,#22107),.UNSPECIFIED.,.F.,.F.,
(4,2,2,2,2,4),(0.,0.374578330850399,0.631956342435387,0.751788955793774,
0.804327350058264,0.853099247911436),.UNSPECIFIED.);
#1054=B_SPLINE_CURVE_WITH_KNOTS('',3,(#22304,#22305,#22306,#22307,#22308,
#22309,#22310,#22311,#22312,#22313),.UNSPECIFIED.,.F.,.F.,(4,2,2,2,4),(0.,
0.0337361869540046,0.0857366303783598,0.186224664796239,0.342354568854618),
 .UNSPECIFIED.);
#1055=B_SPLINE_CURVE_WITH_KNOTS('',3,(#22400,#22401,#22402,#22403,#22404,
#22405,#22406,#22407,#22408,#22409,#22410,#22411),.UNSPECIFIED.,.F.,.F.,
(4,2,2,2,2,4),(0.,0.374578330850087,0.63195634243358,0.751788955791072,
0.804327350055048,0.853099247907485),.UNSPECIFIED.);
#1056=B_SPLINE_CURVE_WITH_KNOTS('',3,(#22509,#22510,#22511,#22512,#22513,
#22514,#22515,#22516,#22517,#22518),.UNSPECIFIED.,.F.,.F.,(4,3,3,4),(0.,
0.0489077955509596,0.146723386652879,0.342354568856692),.UNSPECIFIED.);
#1057=B_SPLINE_CURVE_WITH_KNOTS('',3,(#22580,#22581,#22582,#22583,#22584,
#22585,#22586,#22587,#22588),.UNSPECIFIED.,.F.,.F.,(4,1,1,1,1,1,4),(4.72327004842498,
5.43406096961972,6.1448518911917,6.85564281276368,7.56643373433566,8.27722465590764,
8.97833931241972),.UNSPECIFIED.);
#1058=B_SPLINE_CURVE_WITH_KNOTS('',3,(#22589,#22590,#22591,#22592,#22593),
 .UNSPECIFIED.,.F.,.F.,(4,1,4),(8.97833931241972,8.98801557747962,9.6988064990516),
 .UNSPECIFIED.);
#1059=B_SPLINE_CURVE_WITH_KNOTS('',3,(#22669,#22670,#22671,#22672,#22673,
#22674,#22675,#22676,#22677,#22678,#22679,#22680,#22681,#22682,#22683,#22684,
#22685,#22686,#22687,#22688,#22689,#22690,#22691,#22692,#22693,#22694,#22695,
#22696,#22697,#22698,#22699,#22700,#22701,#22702),.UNSPECIFIED.,.F.,.F.,
(4,3,3,3,3,3,3,3,3,3,3,4),(-2.73245898532687,-2.53728230507538,-2.34210562482388,
-2.14692894457238,-1.95175226432089,-1.82163447748656,-1.69151669065223,
-1.56139890381789,-1.30116333014923,-1.1710455433149,-0.975868863063405,
-0.910819924833371),.UNSPECIFIED.);
#1060=B_SPLINE_CURVE_WITH_KNOTS('',3,(#22705,#22706,#22707,#22708,#22709,
#22710,#22711,#22712,#22713,#22714,#22715,#22716,#22717,#22718,#22719,#22720),
 .UNSPECIFIED.,.F.,.F.,(4,3,3,3,3,4),(-3.64328476398188,-3.3830488272233,
-3.25293085884402,-2.99269492208545,-2.86257695370616,-2.73245898532687),
 .UNSPECIFIED.);
#1061=B_SPLINE_CURVE_WITH_KNOTS('',3,(#22721,#22722,#22723,#22724,#22725,
#22726,#22727,#22728,#22729,#22730,#22731,#22732,#22733,#22734,#22735,#22736),
 .UNSPECIFIED.,.F.,.F.,(4,3,3,3,3,4),(-0.910819924833371,-0.780694259832976,
-0.585520694874732,-0.390347129916488,-0.195173564958244,0.),
 .UNSPECIFIED.);
#1062=B_SPLINE_CURVE_WITH_KNOTS('',3,(#22797,#22798,#22799,#22800,#22801,
#22802,#22803,#22804,#22805,#22806,#22807,#22808),.UNSPECIFIED.,.F.,.F.,
(4,2,2,2,2,4),(-1.80249027418853,-1.70763915321993,-1.57980684458897,-1.45197453595802,
-1.32414222732706,-1.10145879772751),.UNSPECIFIED.);
#1063=B_SPLINE_CURVE_WITH_KNOTS('',3,(#22811,#22812,#22813,#22814,#22815,
#22816,#22817,#22818,#22819,#22820,#22821,#22822),.UNSPECIFIED.,.F.,.F.,
(4,2,2,2,2,4),(1.10145879772751,1.32414222732706,1.45197453595802,1.57980684458897,
1.70763915321993,1.80249027418853),.UNSPECIFIED.);
#1064=B_SPLINE_CURVE_WITH_KNOTS('',3,(#22839,#22840,#22841,#22842),
 .UNSPECIFIED.,.F.,.F.,(4,4),(2.15398534032161,2.26119471261739),
 .UNSPECIFIED.);
#1065=B_SPLINE_CURVE_WITH_KNOTS('',3,(#22843,#22844,#22845,#22846),
 .UNSPECIFIED.,.F.,.F.,(4,4),(-2.26119471261739,-2.15398534032161),
 .UNSPECIFIED.);
#1066=B_SPLINE_CURVE_WITH_KNOTS('',3,(#22872,#22873,#22874,#22875),
 .UNSPECIFIED.,.F.,.F.,(4,4),(0.880397940972402,0.987607313268187),
 .UNSPECIFIED.);
#1067=B_SPLINE_CURVE_WITH_KNOTS('',3,(#22876,#22877,#22878,#22879),
 .UNSPECIFIED.,.F.,.F.,(4,4),(-0.987607313268187,-0.880397940972402),
 .UNSPECIFIED.);
#1068=B_SPLINE_CURVE_WITH_KNOTS('',3,(#22916,#22917,#22918,#22919,#22920,
#22921,#22922,#22923),.UNSPECIFIED.,.F.,.F.,(4,2,1,1,4),(-3.18038929530694,
-3.10150593498916,-2.86856886371248,-2.63563179243579,-2.51916325679745),
 .UNSPECIFIED.);
#1069=B_SPLINE_CURVE_WITH_KNOTS('',3,(#22926,#22927,#22928,#22929,#22930,
#22931,#22932,#22933),.UNSPECIFIED.,.F.,.F.,(4,1,1,2,4),(2.51916325679745,
2.63563179243579,2.86856886371248,3.10150593498916,3.18038929530694),
 .UNSPECIFIED.);
#1070=B_SPLINE_CURVE_WITH_KNOTS('',3,(#22950,#22951,#22952,#22953),
 .UNSPECIFIED.,.F.,.F.,(4,4),(0.552453261527181,0.666064399610344),
 .UNSPECIFIED.);
#1071=B_SPLINE_CURVE_WITH_KNOTS('',3,(#22954,#22955,#22956,#22957),
 .UNSPECIFIED.,.F.,.F.,(4,4),(-0.666064399610344,-0.552453261527181),
 .UNSPECIFIED.);
#1072=B_SPLINE_CURVE_WITH_KNOTS('',3,(#22974,#22975,#22976,#22977),
 .UNSPECIFIED.,.F.,.F.,(4,4),(5.61712090756923,5.7307320456524),
 .UNSPECIFIED.);
#1073=B_SPLINE_CURVE_WITH_KNOTS('',3,(#22978,#22979,#22980,#22981),
 .UNSPECIFIED.,.F.,.F.,(4,4),(-5.7307320456524,-5.61712090756923),
 .UNSPECIFIED.);
#1074=B_SPLINE_CURVE_WITH_KNOTS('',3,(#22988,#22989,#22990,#22991),
 .UNSPECIFIED.,.F.,.F.,(4,4),(0.552453261527181,0.666064399610344),
 .UNSPECIFIED.);
#1075=B_SPLINE_CURVE_WITH_KNOTS('',3,(#22993,#22994,#22995,#22996,#22997,
#22998),.UNSPECIFIED.,.F.,.F.,(4,1,1,4),(-3.18038929530694,-2.8970067073743,
-2.70808498208588,-2.51916325679745),.UNSPECIFIED.);
#1076=B_SPLINE_CURVE_WITH_KNOTS('',3,(#23000,#23001,#23002,#23003),
 .UNSPECIFIED.,.F.,.F.,(4,4),(5.61712090756924,5.7307320456524),
 .UNSPECIFIED.);
#1077=B_SPLINE_CURVE_WITH_KNOTS('',3,(#23073,#23074,#23075,#23076,#23077,
#23078,#23079,#23080,#23081,#23082,#23083,#23084),.UNSPECIFIED.,.F.,.F.,
(4,2,1,1,1,1,1,1,4),(-2.14666332293336,-2.08251480474329,-1.90041544032897,
-1.71831607591465,-1.67279123481106,-1.62726639370748,-1.53621671150032,
-1.354117347086,-1.17201798267167),.UNSPECIFIED.);
#1078=B_SPLINE_CURVE_WITH_KNOTS('',3,(#23088,#23089,#23090,#23091,#23092,
#23093,#23094),.UNSPECIFIED.,.F.,.F.,(4,1,1,1,4),(1.17201798267167,1.354117347086,
1.53621671150032,1.62726639370748,1.65922503472488),.UNSPECIFIED.);
#1079=B_SPLINE_CURVE_WITH_KNOTS('',3,(#23095,#23096,#23097,#23098,#23099,
#23100,#23101,#23102,#23103),.UNSPECIFIED.,.F.,.F.,(4,1,1,1,2,4),(1.65922503472488,
1.67279123481106,1.71831607591465,1.90041544032897,2.08251480474329,2.14666332293336),
 .UNSPECIFIED.);
#1080=B_SPLINE_CURVE_WITH_KNOTS('',3,(#23120,#23121,#23122,#23123),
 .UNSPECIFIED.,.F.,.F.,(4,4),(-2.37317063593509,-2.29711532831763),
 .UNSPECIFIED.);
#1081=B_SPLINE_CURVE_WITH_KNOTS('',3,(#23124,#23125,#23126,#23127),
 .UNSPECIFIED.,.F.,.F.,(4,4),(2.29711532831763,2.37317063593509),
 .UNSPECIFIED.);
#1082=B_SPLINE_CURVE_WITH_KNOTS('',3,(#23153,#23154,#23155,#23156),
 .UNSPECIFIED.,.F.,.F.,(4,4),(2.29711532831763,2.37317063593509),
 .UNSPECIFIED.);
#1083=B_SPLINE_CURVE_WITH_KNOTS('',3,(#23157,#23158,#23159,#23160),
 .UNSPECIFIED.,.F.,.F.,(4,4),(-2.37317063593509,-2.29711532831763),
 .UNSPECIFIED.);
#1084=B_SPLINE_CURVE_WITH_KNOTS('',3,(#23197,#23198,#23199,#23200,#23201,
#23202,#23203,#23204),.UNSPECIFIED.,.F.,.F.,(4,2,1,1,4),(-1.80249027418852,
-1.70763915321993,-1.46516701102296,-1.34393093992448,-1.10145879772751),
 .UNSPECIFIED.);
#1085=B_SPLINE_CURVE_WITH_KNOTS('',3,(#23207,#23208,#23209,#23210,#23211,
#23212,#23213,#23214),.UNSPECIFIED.,.F.,.F.,(4,1,1,2,4),(1.10145879772751,
1.34393093992448,1.46516701102296,1.70763915321993,1.80249027418852),
 .UNSPECIFIED.);
#1086=B_SPLINE_CURVE_WITH_KNOTS('',3,(#23231,#23232,#23233,#23234),
 .UNSPECIFIED.,.F.,.F.,(4,4),(2.1539853403216,2.26119471261739),
 .UNSPECIFIED.);
#1087=B_SPLINE_CURVE_WITH_KNOTS('',3,(#23235,#23236,#23237,#23238),
 .UNSPECIFIED.,.F.,.F.,(4,4),(-2.26119471261739,-2.1539853403216),
 .UNSPECIFIED.);
#1088=B_SPLINE_CURVE_WITH_KNOTS('',3,(#23255,#23256,#23257,#23258),
 .UNSPECIFIED.,.F.,.F.,(4,4),(0.880397940972402,0.987607313268191),
 .UNSPECIFIED.);
#1089=B_SPLINE_CURVE_WITH_KNOTS('',3,(#23259,#23260,#23261,#23262),
 .UNSPECIFIED.,.F.,.F.,(4,4),(-0.987607313268191,-0.880397940972402),
 .UNSPECIFIED.);
#1090=B_SPLINE_CURVE_WITH_KNOTS('',3,(#23329,#23330,#23331,#23332,#23333,
#23334,#23335,#23336,#23337,#23338),.UNSPECIFIED.,.F.,.F.,(4,1,1,1,1,2,
4),(-3.25446481014654,-3.07261070349882,-3.01199266794958,-2.89075659685109,
-2.76952052575261,-2.64828445465413,-2.55343333368553),.UNSPECIFIED.);
#1091=B_SPLINE_CURVE_WITH_KNOTS('',3,(#23341,#23342,#23343,#23344,#23345,
#23346,#23347,#23348,#23349,#23350),.UNSPECIFIED.,.F.,.F.,(4,2,1,1,1,1,
4),(2.55343333368553,2.64828445465413,2.76952052575261,2.89075659685109,
3.01199266794958,3.07261070349882,3.25446481014654),.UNSPECIFIED.);
#1092=B_SPLINE_CURVE_WITH_KNOTS('',3,(#23367,#23368,#23369,#23370),
 .UNSPECIFIED.,.F.,.F.,(4,4),(5.29557799391139,5.40278736620718),
 .UNSPECIFIED.);
#1093=B_SPLINE_CURVE_WITH_KNOTS('',3,(#23371,#23372,#23373,#23374),
 .UNSPECIFIED.,.F.,.F.,(4,4),(-5.40278736620718,-5.29557799391139),
 .UNSPECIFIED.);
#1094=B_SPLINE_CURVE_WITH_KNOTS('',3,(#23399,#23400,#23401,#23402),
 .UNSPECIFIED.,.F.,.F.,(4,4),(4.0219905945622,4.12919996685799),
 .UNSPECIFIED.);
#1095=B_SPLINE_CURVE_WITH_KNOTS('',3,(#23403,#23404,#23405,#23406),
 .UNSPECIFIED.,.F.,.F.,(4,4),(-4.12919996685799,-4.0219905945622),
 .UNSPECIFIED.);
#1096=B_SPLINE_CURVE_WITH_KNOTS('',3,(#23435,#23436,#23437,#23438,#23439,
#23440),.UNSPECIFIED.,.F.,.F.,(4,1,1,4),(2.51916325679745,2.70808498208588,
2.8970067073743,3.18038929530694),.UNSPECIFIED.);
#1097=B_SPLINE_CURVE_WITH_KNOTS('',3,(#23457,#23458,#23459,#23460),
 .UNSPECIFIED.,.F.,.F.,(4,4),(-0.666064399610344,-0.552453261527181),
 .UNSPECIFIED.);
#1098=B_SPLINE_CURVE_WITH_KNOTS('',3,(#23477,#23478,#23479,#23480),
 .UNSPECIFIED.,.F.,.F.,(4,4),(-5.7307320456524,-5.61712090756924),
 .UNSPECIFIED.);
#1099=B_SPLINE_CURVE_WITH_KNOTS('',3,(#23519,#23520,#23521,#23522,#23523,
#23524),.UNSPECIFIED.,.F.,.F.,(4,1,1,4),(-3.25446481014654,-3.05417010258625,
-2.85387539502596,-2.55343333368552),.UNSPECIFIED.);
#1100=B_SPLINE_CURVE_WITH_KNOTS('',3,(#23527,#23528,#23529,#23530,#23531,
#23532),.UNSPECIFIED.,.F.,.F.,(4,1,1,4),(2.55343333368552,2.85387539502596,
3.05417010258625,3.25446481014654),.UNSPECIFIED.);
#1101=B_SPLINE_CURVE_WITH_KNOTS('',3,(#23549,#23550,#23551,#23552),
 .UNSPECIFIED.,.F.,.F.,(4,4),(-0.987607313268191,-0.880397940972406),
 .UNSPECIFIED.);
#1102=B_SPLINE_CURVE_WITH_KNOTS('',3,(#23553,#23554,#23555,#23556),
 .UNSPECIFIED.,.F.,.F.,(4,4),(0.880397940972406,0.987607313268191),
 .UNSPECIFIED.);
#1103=B_SPLINE_CURVE_WITH_KNOTS('',3,(#23582,#23583,#23584,#23585),
 .UNSPECIFIED.,.F.,.F.,(4,4),(-2.26119471261739,-2.1539853403216),
 .UNSPECIFIED.);
#1104=B_SPLINE_CURVE_WITH_KNOTS('',3,(#23586,#23587,#23588,#23589),
 .UNSPECIFIED.,.F.,.F.,(4,4),(2.1539853403216,2.26119471261739),
 .UNSPECIFIED.);
#1105=B_SPLINE_CURVE_WITH_KNOTS('',3,(#23646,#23647,#23648,#23649,#23650,
#23651,#23652,#23653,#23654,#23655,#23656,#23657,#23658),.UNSPECIFIED.,
 .F.,.F.,(4,2,1,1,1,1,1,2,4),(-2.14666332293336,-1.94145675409637,-1.80039870344944,
-1.65934065280252,-1.58881162747905,-1.51828260215559,-1.37722455150867,
-1.23616650086174,-1.17201798267168),.UNSPECIFIED.);
#1106=B_SPLINE_CURVE_WITH_KNOTS('',3,(#23662,#23663,#23664,#23665,#23666,
#23667,#23668,#23669,#23670),.UNSPECIFIED.,.F.,.F.,(4,2,1,1,1,4),(1.17201798267168,
1.23616650086174,1.37722455150867,1.51828260215559,1.58881162747905,1.65930014766736),
 .UNSPECIFIED.);
#1107=B_SPLINE_CURVE_WITH_KNOTS('',3,(#23671,#23672,#23673,#23674,#23675,
#23676,#23677,#23678),.UNSPECIFIED.,.F.,.F.,(4,1,1,2,4),(1.65930014766736,
1.65934065280252,1.80039870344944,1.94145675409637,2.14666332293336),
 .UNSPECIFIED.);
#1108=B_SPLINE_CURVE_WITH_KNOTS('',3,(#23695,#23696,#23697,#23698),
 .UNSPECIFIED.,.F.,.F.,(4,4),(-2.37317063593509,-2.29711532831763),
 .UNSPECIFIED.);
#1109=B_SPLINE_CURVE_WITH_KNOTS('',3,(#23699,#23700,#23701,#23702),
 .UNSPECIFIED.,.F.,.F.,(4,4),(2.29711532831763,2.37317063593509),
 .UNSPECIFIED.);
#1110=B_SPLINE_CURVE_WITH_KNOTS('',3,(#23719,#23720,#23721,#23722),
 .UNSPECIFIED.,.F.,.F.,(4,4),(2.29711532831763,2.37317063593509),
 .UNSPECIFIED.);
#1111=B_SPLINE_CURVE_WITH_KNOTS('',3,(#23723,#23724,#23725,#23726),
 .UNSPECIFIED.,.F.,.F.,(4,4),(-2.37317063593509,-2.29711532831763),
 .UNSPECIFIED.);
#1112=B_SPLINE_CURVE_WITH_KNOTS('',3,(#23759,#23760,#23761,#23762),
 .UNSPECIFIED.,.F.,.F.,(4,4),(-1.,0.),.UNSPECIFIED.);
#1113=B_SPLINE_CURVE_WITH_KNOTS('',3,(#23764,#23765,#23766,#23767),
 .UNSPECIFIED.,.F.,.F.,(4,4),(-0.626198664785115,-0.624325079343485),
 .UNSPECIFIED.);
#1114=B_SPLINE_CURVE_WITH_KNOTS('',3,(#23769,#23770,#23771,#23772),
 .UNSPECIFIED.,.F.,.F.,(4,4),(-1.,0.),.UNSPECIFIED.);
#1115=B_SPLINE_CURVE_WITH_KNOTS('',3,(#23773,#23774,#23775,#23776),
 .UNSPECIFIED.,.F.,.F.,(4,4),(0.624325079342602,0.626198664785115),
 .UNSPECIFIED.);
#1116=B_SPLINE_CURVE_WITH_KNOTS('',3,(#23818,#23819,#23820,#23821,#23822,
#23823,#23824,#23825,#23826,#23827,#23828,#23829,#23830),.UNSPECIFIED.,
 .F.,.F.,(4,3,3,3,4),(-0.624325079343337,-0.380129337103437,-0.301935532403907,
-0.237254059228539,-0.209869946944685),.UNSPECIFIED.);
#1117=B_SPLINE_CURVE_WITH_KNOTS('',3,(#23833,#23834,#23835,#23836,#23837,
#23838,#23839,#23840,#23841,#23842),.UNSPECIFIED.,.F.,.F.,(4,2,2,2,4),(0.209869946944685,
0.237254059228639,0.301935532404242,0.380129337104056,0.624325079343485),
 .UNSPECIFIED.);
#1118=B_SPLINE_CURVE_WITH_KNOTS('',3,(#23860,#23861,#23862,#23863),
 .UNSPECIFIED.,.F.,.F.,(4,4),(0.626198664785115,0.626730655849092),
 .UNSPECIFIED.);
#1119=B_SPLINE_CURVE_WITH_KNOTS('',3,(#23865,#23866,#23867,#23868),
 .UNSPECIFIED.,.F.,.F.,(4,4),(0.,0.40461689765448),.UNSPECIFIED.);
#1120=B_SPLINE_CURVE_WITH_KNOTS('',3,(#23870,#23871,#23872,#23873),
 .UNSPECIFIED.,.F.,.F.,(4,4),(0.40461689765448,1.),.UNSPECIFIED.);
#1121=B_SPLINE_CURVE_WITH_KNOTS('',3,(#23874,#23875,#23876,#23877),
 .UNSPECIFIED.,.F.,.F.,(4,4),(-0.626730655849168,-0.626198664785115),
 .UNSPECIFIED.);
#1122=B_SPLINE_CURVE_WITH_KNOTS('',3,(#23881,#23882,#23883,#23884,#23885,
#23886,#23887,#23888,#23889,#23890,#23891,#23892),.UNSPECIFIED.,.F.,.F.,
(4,2,2,2,2,4),(0.138038496450912,0.161248355370673,0.204799871014317,0.238374998155151,
0.276615810149267,0.305604882133989),.UNSPECIFIED.);
#1123=B_SPLINE_CURVE_WITH_KNOTS('',3,(#23914,#23915,#23916,#23917),
 .UNSPECIFIED.,.F.,.F.,(4,4),(-1.50825556499841,-1.48736624018428),
 .UNSPECIFIED.);
#1124=B_SPLINE_CURVE_WITH_KNOTS('',3,(#23918,#23919,#23920,#23921),
 .UNSPECIFIED.,.F.,.F.,(4,4),(1.48736624018428,1.50825556499841),
 .UNSPECIFIED.);
#1125=B_SPLINE_CURVE_WITH_KNOTS('',3,(#23939,#23940,#23941,#23942),
 .UNSPECIFIED.,.F.,.F.,(4,4),(0.,1.),.UNSPECIFIED.);
#1126=B_SPLINE_CURVE_WITH_KNOTS('',3,(#23943,#23944,#23945,#23946),
 .UNSPECIFIED.,.F.,.F.,(4,4),(-1.,0.),.UNSPECIFIED.);
#1127=B_SPLINE_CURVE_WITH_KNOTS('',3,(#23949,#23950,#23951,#23952,#23953,
#23954,#23955,#23956,#23957,#23958),.UNSPECIFIED.,.F.,.F.,(4,2,2,2,4),(0.332744846717523,
0.350102619564171,0.400216488498811,0.450330357433451,0.50044422636809),
 .UNSPECIFIED.);
#1128=B_SPLINE_CURVE_WITH_KNOTS('',3,(#23962,#23963,#23964,#23965,#23966,
#23967,#23968,#23969,#23970,#23971,#23972,#23973,#23974,#23975,#23976,#23977),
 .UNSPECIFIED.,.F.,.F.,(4,2,2,2,2,2,2,4),(0.,0.00679055346363672,0.0146345859059421,
0.0291055700835612,0.0660529231384144,0.0914869265287218,0.111277934482435,
0.124254482609582),.UNSPECIFIED.);
#1129=B_SPLINE_CURVE_WITH_KNOTS('',3,(#24003,#24004,#24005,#24006),
 .UNSPECIFIED.,.F.,.F.,(4,4),(-1.,0.),.UNSPECIFIED.);
#1130=B_SPLINE_CURVE_WITH_KNOTS('',3,(#24008,#24009,#24010,#24011,#24012),
 .UNSPECIFIED.,.F.,.F.,(4,1,4),(0.,0.000208214441420064,0.000485833696646816),
 .UNSPECIFIED.);
#1131=B_SPLINE_CURVE_WITH_KNOTS('',3,(#24014,#24015,#24016,#24017),
 .UNSPECIFIED.,.F.,.F.,(4,4),(-1.,-0.37748786671169),.UNSPECIFIED.);
#1132=B_SPLINE_CURVE_WITH_KNOTS('',3,(#24019,#24020,#24021,#24022),
 .UNSPECIFIED.,.F.,.F.,(4,4),(-0.37748786671169,0.),.UNSPECIFIED.);
#1133=B_SPLINE_CURVE_WITH_KNOTS('',3,(#24023,#24024,#24025,#24026,#24027),
 .UNSPECIFIED.,.F.,.F.,(4,1,4),(-0.000485833696646816,-0.000208214441420064,
0.),.UNSPECIFIED.);
#1134=B_SPLINE_CURVE_WITH_KNOTS('',3,(#24052,#24053,#24054,#24055),
 .UNSPECIFIED.,.F.,.F.,(4,4),(-1.,0.),.UNSPECIFIED.);
#1135=B_SPLINE_CURVE_WITH_KNOTS('',3,(#24111,#24112,#24113,#24114,#24115,
#24116,#24117,#24118,#24119,#24120,#24121,#24122),.UNSPECIFIED.,.F.,.F.,
(4,2,2,2,2,4),(0.00166298225714781,0.120337282444558,0.218409540651057,
0.287813854984672,0.345224711421131,0.369530672027591),.UNSPECIFIED.);
#1136=B_SPLINE_CURVE_WITH_KNOTS('',3,(#24125,#24126,#24127,#24128,#24129,
#24130,#24131,#24132,#24133,#24134,#24135,#24136),.UNSPECIFIED.,.F.,.F.,
(4,2,2,2,2,4),(-0.369530672027591,-0.345224711421131,-0.287813854984672,
-0.218409540651057,-0.120337282444558,-0.00166298225714781),
 .UNSPECIFIED.);
#1137=B_SPLINE_CURVE_WITH_KNOTS('',3,(#24144,#24145,#24146,#24147,#24148,
#24149,#24150,#24151,#24152,#24153,#24154,#24155),.UNSPECIFIED.,.F.,.F.,
(4,2,2,2,2,4),(0.519582720249636,0.548571792234358,0.586812604228477,0.620387731369311,
0.663939247012956,0.687149105932712),.UNSPECIFIED.);
#1138=B_SPLINE_CURVE_WITH_KNOTS('',3,(#24173,#24174,#24175,#24176),
 .UNSPECIFIED.,.F.,.F.,(4,4),(4.77492974218118,4.7958190669953),
 .UNSPECIFIED.);
#1139=B_SPLINE_CURVE_WITH_KNOTS('',3,(#24177,#24178,#24179,#24180),
 .UNSPECIFIED.,.F.,.F.,(4,4),(-4.7958190669953,-4.77492974218118),
 .UNSPECIFIED.);
#1140=B_SPLINE_CURVE_WITH_KNOTS('',3,(#24198,#24199,#24200,#24201),
 .UNSPECIFIED.,.F.,.F.,(4,4),(0.,1.),.UNSPECIFIED.);
#1141=B_SPLINE_CURVE_WITH_KNOTS('',3,(#24202,#24203,#24204,#24205),
 .UNSPECIFIED.,.F.,.F.,(4,4),(-1.,0.),.UNSPECIFIED.);
#1142=B_SPLINE_CURVE_WITH_KNOTS('',3,(#24301,#24302,#24303,#24304,#24305,
#24306,#24307,#24308,#24309,#24310,#24311,#24312,#24313,#24314),
 .UNSPECIFIED.,.F.,.F.,(4,1,1,1,1,1,1,1,1,1,1,4),(-2.80995821199303,-2.67614471704543,
-2.54233748119315,-2.40853024534088,-2.14091577363634,-1.96250612583331,
-1.78409647803028,-1.60568683022725,-1.42727718242423,-1.2488675346212,
-1.07045788681817,-0.936655001901496),.UNSPECIFIED.);
#1143=B_SPLINE_CURVE_WITH_KNOTS('',3,(#24317,#24318,#24319,#24320,#24321,
#24322,#24323,#24324),.UNSPECIFIED.,.F.,.F.,(4,1,1,1,1,4),(-3.74660260386359,
-3.61279536801132,-3.47898813215905,-3.21137366045451,-2.94375918874997,
-2.80995821199303),.UNSPECIFIED.);
#1144=B_SPLINE_CURVE_WITH_KNOTS('',3,(#24325,#24326,#24327,#24328,#24329,
#24330,#24331,#24332),.UNSPECIFIED.,.F.,.F.,(4,1,1,1,1,4),(-0.936655001901496,
-0.802843415113627,-0.535228943409085,-0.267614471704543,-0.133807235852271,
0.),.UNSPECIFIED.);
#1145=B_SPLINE_CURVE_WITH_KNOTS('',3,(#24445,#24446,#24447,#24448,#24449,
#24450,#24451,#24452,#24453,#24454,#24455,#24456,#24457,#24458,#24459,#24460,
#24461,#24462,#24463,#24464,#24465,#24466),.UNSPECIFIED.,.T.,.F.,(4,1,1,
1,1,1,1,1,1,1,1,1,1,1,1,1,1,1,1,4),(0.,0.133807235852271,0.267614471704543,
0.535228943409085,0.802843415113627,1.07045788681817,1.2488675346212,1.42727718242423,
1.60568683022725,1.78409647803028,1.96250612583331,2.14091577363634,2.40853024534088,
2.54233748119315,2.67614471704543,2.94375918874997,3.21137366045451,3.47898813215905,
3.61279536801132,3.74660260386359),.UNSPECIFIED.);
#1146=B_SPLINE_CURVE_WITH_KNOTS('',3,(#24478,#24479,#24480,#24481,#24482,
#24483,#24484,#24485,#24486,#24487,#24488,#24489,#24490,#24491),
 .UNSPECIFIED.,.F.,.F.,(4,2,2,2,2,2,4),(-0.345305288041167,-0.344620712595134,
-0.226569517485857,-0.15131577954814,-0.0758841034235322,-0.030282394435752,
0.),.UNSPECIFIED.);
#1147=B_SPLINE_CURVE_WITH_KNOTS('',3,(#24505,#24506,#24507,#24508,#24509,
#24510,#24511,#24512,#24513,#24514,#24515,#24516,#24517,#24518),
 .UNSPECIFIED.,.F.,.F.,(4,2,2,2,2,2,4),(-0.422554374321187,-0.385423821412686,
-0.329509594686649,-0.237019555721844,-0.144747694460498,0.,0.000839387766042462),
 .UNSPECIFIED.);
#1148=B_SPLINE_CURVE_WITH_KNOTS('',3,(#24531,#24532,#24533,#24534,#24535,
#24536,#24537,#24538,#24539,#24540,#24541,#24542,#24543,#24544),
 .UNSPECIFIED.,.F.,.F.,(4,2,2,2,2,2,4),(-0.345305322448276,-0.344620746646918,
-0.22656951748443,-0.151315779547605,-0.0758841034234829,-0.030282394435745,
0.),.UNSPECIFIED.);
#1149=B_SPLINE_CURVE_WITH_KNOTS('',3,(#24566,#24567,#24568,#24569,#24570,
#24571,#24572,#24573,#24574,#24575,#24576,#24577,#24578,#24579),
 .UNSPECIFIED.,.F.,.F.,(4,2,2,2,2,2,4),(-0.351506503283319,-0.286559194099349,
-0.217668322783822,-0.136952361437555,-0.0679759511705759,0.,0.000711948788676417),
 .UNSPECIFIED.);
#1150=B_SPLINE_CURVE_WITH_KNOTS('',3,(#24594,#24595,#24596,#24597,#24598,
#24599,#24600,#24601,#24602,#24603,#24604,#24605,#24606,#24607),
 .UNSPECIFIED.,.F.,.F.,(4,2,2,2,2,2,4),(-0.350131750560411,-0.349424019690355,
-0.281850788688661,-0.213283025920958,-0.133045262492339,-0.0645625319046002,
0.),.UNSPECIFIED.);
#1151=B_SPLINE_CURVE_WITH_KNOTS('',3,(#24767,#24768,#24769,#24770,#24771,
#24772,#24773,#24774,#24775,#24776,#24777,#24778,#24779,#24780,#24781,#24782,
#24783,#24784,#24785,#24786,#24787,#24788,#24789,#24790,#24791,#24792,#24793,
#24794,#24795,#24796,#24797,#24798,#24799,#24800,#24801,#24802,#24803,#24804,
#24805,#24806,#24807,#24808,#24809,#24810,#24811,#24812,#24813,#24814,#24815,
#24816,#24817,#24818,#24819,#24820,#24821,#24822,#24823,#24824,#24825,#24826,
#24827,#24828,#24829,#24830,#24831,#24832,#24833,#24834,#24835,#24836,#24837,
#24838,#24839,#24840,#24841,#24842,#24843,#24844,#24845,#24846,#24847,#24848,
#24849,#24850,#24851,#24852,#24853,#24854,#24855,#24856,#24857,#24858,#24859,
#24860,#24861,#24862,#24863,#24864,#24865,#24866,#24867,#24868,#24869,#24870,
#24871,#24872,#24873,#24874,#24875,#24876,#24877,#24878,#24879,#24880,#24881,
#24882,#24883,#24884,#24885,#24886,#24887,#24888,#24889,#24890,#24891,#24892,
#24893,#24894,#24895,#24896,#24897,#24898,#24899,#24900,#24901,#24902,#24903,
#24904,#24905,#24906,#24907,#24908,#24909,#24910,#24911,#24912,#24913,#24914,
#24915,#24916,#24917,#24918,#24919,#24920,#24921,#24922,#24923,#24924,#24925,
#24926,#24927,#24928,#24929,#24930,#24931,#24932,#24933,#24934,#24935,#24936,
#24937,#24938,#24939,#24940,#24941,#24942,#24943,#24944,#24945,#24946,#24947,
#24948,#24949,#24950,#24951,#24952,#24953,#24954,#24955,#24956,#24957,#24958,
#24959,#24960,#24961,#24962,#24963,#24964,#24965,#24966,#24967,#24968,#24969,
#24970,#24971,#24972,#24973,#24974,#24975,#24976,#24977,#24978,#24979,#24980,
#24981,#24982,#24983,#24984,#24985,#24986,#24987,#24988,#24989,#24990,#24991,
#24992,#24993,#24994,#24995,#24996,#24997,#24998,#24999,#25000,#25001,#25002,
#25003,#25004,#25005,#25006,#25007,#25008,#25009,#25010,#25011,#25012,#25013,
#25014,#25015,#25016,#25017,#25018,#25019),.UNSPECIFIED.,.F.,.F.,(4,3,3,
3,3,3,3,3,3,3,3,3,3,3,3,3,3,3,3,3,3,3,3,3,3,3,3,3,3,3,3,3,3,3,3,3,3,3,3,
3,3,3,3,3,3,3,3,3,3,3,3,3,3,3,3,3,3,3,3,3,3,3,3,3,3,3,3,3,3,3,3,3,3,3,3,
3,3,3,3,3,3,3,3,3,4),(0.,0.0813280369871104,0.10426271137412,0.17724565415719,
0.248684089577596,0.320122524998002,0.388171850673652,0.45433223954272,
0.496422333197618,0.555732946496683,0.613636795430242,0.640021394627608,
0.696656237449289,0.753087155105956,0.808915529598096,0.836983440014268,
0.892384452514873,0.947440153385303,0.95982385581978,1.01461986638795,1.06994040744583,
1.12583018879548,1.17176297454938,1.23015322407112,1.27982518853794,1.33869000601364,
1.39774705874962,1.4567876494499,1.49291289003645,1.55328529142365,1.5998485198889,
1.66004066589129,1.71941954967881,1.77418606762871,1.83221046372469,1.88941828995785,
1.91970052834762,1.9760468885945,2.032160295288,2.08764355038908,2.11139064429874,
2.13283348679512,2.18717034576841,2.24227858706577,2.29844665483361,2.35506564452401,
2.41206805172476,2.44465988147568,2.51246843122597,2.55981452659546,2.62802745211438,
2.70048101976627,2.77293458741816,2.82461261529351,2.88939162661952,2.95507054101926,
2.98614701351453,3.05100710484421,3.10476710153347,3.17625736575752,3.19959679788099,
3.26972372420938,3.3376297735848,3.40411528115335,3.46846403910524,3.51930648273169,
3.5202225802945,3.57838132493156,3.63653714411098,3.69409893873786,3.75108640250181,
3.80705542924498,3.83890564683775,3.87319766720952,3.93090365877466,3.98960105332232,
4.04855689348964,4.10738895498192,4.15897712336674,4.21313376356879,4.27400032548969,
4.33648185529254,4.39979751513143,4.46403159890671,4.47914967830435),
 .UNSPECIFIED.);
#1152=B_SPLINE_CURVE_WITH_KNOTS('',3,(#25069,#25070,#25071,#25072,#25073,
#25074,#25075,#25076),.UNSPECIFIED.,.F.,.F.,(4,1,1,1,1,4),(0.,0.213141959635737,
0.426283919271474,0.852567838542947,1.06570979817868,1.49199371745016),
 .UNSPECIFIED.);
#1153=B_SPLINE_CURVE_WITH_KNOTS('',3,(#25084,#25085,#25086,#25087,#25088,
#25089,#25090,#25091,#25092,#25093,#25094,#25095,#25096,#25097),
 .UNSPECIFIED.,.F.,.F.,(4,2,2,2,2,2,4),(0.37662094331532,0.433515090571885,
0.499087916949629,0.586028073495358,0.673570485757201,0.765226500919176,
0.766118331324739),.UNSPECIFIED.);
#1154=B_SPLINE_CURVE_WITH_KNOTS('',3,(#25108,#25109,#25110,#25111,#25112,
#25113,#25114,#25115,#25116,#25117,#25118,#25119,#25120,#25121,#25122,#25123,
#25124,#25125,#25126,#25127),.UNSPECIFIED.,.F.,.F.,(4,2,2,2,2,2,2,2,2,4),
(0.422785857755809,0.43703384117159,0.463320009434893,0.49635128790697,
0.541631933053045,0.566268869107166,0.583621071618297,0.593824785751523,
0.601681049890584,0.601998413219366),.UNSPECIFIED.);
#1155=B_SPLINE_CURVE_WITH_KNOTS('',3,(#25131,#25132,#25133,#25134,#25135,
#25136,#25137,#25138,#25139,#25140,#25141,#25142,#25143,#25144),
 .UNSPECIFIED.,.F.,.F.,(4,2,2,2,2,2,4),(-0.000892803052402962,0.,0.0917559770331036,
0.179393864789738,0.266428839998198,0.3320731814037,0.38902937854808),
 .UNSPECIFIED.);
#1156=B_SPLINE_CURVE_WITH_KNOTS('',3,(#25158,#25159,#25160,#25161,#25162,
#25163,#25164,#25165,#25166,#25167,#25168,#25169,#25170,#25171),
 .UNSPECIFIED.,.F.,.F.,(4,2,2,2,2,2,4),(0.376620943315501,0.433515090572235,
0.499087916950171,0.586028073496191,0.673570485758674,0.765226500920609,
0.766118331324419),.UNSPECIFIED.);
#1157=B_SPLINE_CURVE_WITH_KNOTS('',3,(#25175,#25176,#25177,#25178,#25179,
#25180,#25181,#25182,#25183,#25184,#25185,#25186,#25187,#25188),
 .UNSPECIFIED.,.F.,.F.,(4,2,2,2,2,2,4),(-0.00089280305197105,0.,0.0917559770332232,
0.17939386478995,0.266428839998158,0.332073181403452,0.389029378547644),
 .UNSPECIFIED.);
#1158=B_SPLINE_CURVE_WITH_KNOTS('',3,(#25201,#25202,#25203,#25204,#25205,
#25206,#25207,#25208,#25209,#25210,#25211,#25212,#25213,#25214),
 .UNSPECIFIED.,.F.,.F.,(4,2,2,2,2,2,4),(0.376620943315551,0.433515090572292,
0.499087916950247,0.586028073496283,0.673570485758794,0.765226500920732,
0.766118331324744),.UNSPECIFIED.);
#1159=B_SPLINE_CURVE_WITH_KNOTS('',3,(#25218,#25219,#25220,#25221,#25222,
#25223,#25224,#25225,#25226,#25227,#25228,#25229,#25230,#25231),
 .UNSPECIFIED.,.F.,.F.,(4,2,2,2,2,2,4),(-0.000892803051768479,0.,0.0917559770332231,
0.179393864789949,0.266428839998158,0.332073181403451,0.389029378547642),
 .UNSPECIFIED.);
#1160=B_SPLINE_CURVE_WITH_KNOTS('',3,(#25301,#25302,#25303,#25304,#25305,
#25306,#25307,#25308,#25309,#25310),.UNSPECIFIED.,.F.,.F.,(4,2,2,2,4),(0.500444226368088,
0.550558095302727,0.600671964237367,0.650785833172007,0.66814360601866),
 .UNSPECIFIED.);
#1161=B_SPLINE_CURVE_WITH_KNOTS('',3,(#25316,#25317,#25318,#25319,#25320,
#25321,#25322,#25323,#25324,#25325,#25326,#25327,#25328,#25329),
 .UNSPECIFIED.,.F.,.F.,(4,2,2,2,2,2,4),(-0.422554267641051,-0.385423725942617,
-0.329509516097576,-0.237019505055533,-0.1447476716502,0.,0.000839387731405013),
 .UNSPECIFIED.);
#1162=B_SPLINE_CURVE_WITH_KNOTS('',3,(#25752,#25753,#25754,#25755),
 .UNSPECIFIED.,.F.,.F.,(4,4),(-0.082197241799306,0.),.UNSPECIFIED.);
#1163=B_SPLINE_CURVE_WITH_KNOTS('',3,(#25766,#25767,#25768,#25769),
 .UNSPECIFIED.,.F.,.F.,(4,4),(-0.0821909663426025,0.),.UNSPECIFIED.);
#1164=B_SPLINE_CURVE_WITH_KNOTS('',3,(#25817,#25818,#25819,#25820),
 .UNSPECIFIED.,.F.,.F.,(4,4),(-0.0821972417993003,0.),.UNSPECIFIED.);
#1165=B_SPLINE_CURVE_WITH_KNOTS('',3,(#25831,#25832,#25833,#25834),
 .UNSPECIFIED.,.F.,.F.,(4,4),(-0.0821909663425251,0.),.UNSPECIFIED.);
#1166=B_SPLINE_CURVE_WITH_KNOTS('',3,(#25882,#25883,#25884,#25885),
 .UNSPECIFIED.,.F.,.F.,(4,4),(-0.0821972417992908,0.),.UNSPECIFIED.);
#1167=B_SPLINE_CURVE_WITH_KNOTS('',3,(#25896,#25897,#25898,#25899),
 .UNSPECIFIED.,.F.,.F.,(4,4),(-0.0821909663425343,0.),.UNSPECIFIED.);
#1168=B_SPLINE_CURVE_WITH_KNOTS('',3,(#25947,#25948,#25949,#25950),
 .UNSPECIFIED.,.F.,.F.,(4,4),(-0.0821972417992827,0.),.UNSPECIFIED.);
#1169=B_SPLINE_CURVE_WITH_KNOTS('',3,(#25961,#25962,#25963,#25964),
 .UNSPECIFIED.,.F.,.F.,(4,4),(-0.0821909663425014,0.),.UNSPECIFIED.);
#1170=B_SPLINE_CURVE_WITH_KNOTS('',3,(#26041,#26042,#26043,#26044),
 .UNSPECIFIED.,.F.,.F.,(4,4),(-0.0821909663426067,0.),.UNSPECIFIED.);
#1171=B_SPLINE_CURVE_WITH_KNOTS('',3,(#26152,#26153,#26154,#26155),
 .UNSPECIFIED.,.F.,.F.,(4,4),(-0.0821972417992939,0.),.UNSPECIFIED.);
#1172=B_SPLINE_CURVE_WITH_KNOTS('',3,(#26163,#26164,#26165,#26166),
 .UNSPECIFIED.,.F.,.F.,(4,4),(-0.0821909663424864,0.),.UNSPECIFIED.);
#1173=B_SPLINE_CURVE_WITH_KNOTS('',3,(#26206,#26207,#26208,#26209),
 .UNSPECIFIED.,.F.,.F.,(4,4),(-0.0821972417992863,0.),.UNSPECIFIED.);
#1174=B_SPLINE_CURVE_WITH_KNOTS('',3,(#26217,#26218,#26219,#26220),
 .UNSPECIFIED.,.F.,.F.,(4,4),(-0.0821909663425319,0.),.UNSPECIFIED.);
#1175=B_SPLINE_CURVE_WITH_KNOTS('',3,(#26368,#26369,#26370,#26371),
 .UNSPECIFIED.,.F.,.F.,(4,4),(-0.0821972417993165,0.),.UNSPECIFIED.);
#1176=B_SPLINE_CURVE_WITH_KNOTS('',3,(#26379,#26380,#26381,#26382),
 .UNSPECIFIED.,.F.,.F.,(4,4),(-0.0821909663426151,0.),.UNSPECIFIED.);
#1177=B_SPLINE_CURVE_WITH_KNOTS('',3,(#26415,#26416,#26417,#26418),
 .UNSPECIFIED.,.F.,.F.,(4,4),(-0.0821972417992918,0.),.UNSPECIFIED.);
#1178=B_SPLINE_CURVE_WITH_KNOTS('',3,(#26426,#26427,#26428,#26429),
 .UNSPECIFIED.,.F.,.F.,(4,4),(-0.0821909663425472,0.),.UNSPECIFIED.);
#1179=B_SPLINE_CURVE_WITH_KNOTS('',3,(#26462,#26463,#26464,#26465),
 .UNSPECIFIED.,.F.,.F.,(4,4),(-0.0821972417992798,0.),.UNSPECIFIED.);
#1180=B_SPLINE_CURVE_WITH_KNOTS('',3,(#26473,#26474,#26475,#26476),
 .UNSPECIFIED.,.F.,.F.,(4,4),(-0.0821909663425245,0.),.UNSPECIFIED.);
#1181=B_SPLINE_CURVE_WITH_KNOTS('',3,(#26509,#26510,#26511,#26512),
 .UNSPECIFIED.,.F.,.F.,(4,4),(-0.082197241799281,0.),.UNSPECIFIED.);
#1182=B_SPLINE_CURVE_WITH_KNOTS('',3,(#26520,#26521,#26522,#26523),
 .UNSPECIFIED.,.F.,.F.,(4,4),(-0.0821909663425156,0.),.UNSPECIFIED.);
#1183=B_SPLINE_CURVE_WITH_KNOTS('',3,(#26556,#26557,#26558,#26559),
 .UNSPECIFIED.,.F.,.F.,(4,4),(-0.0821972417993007,0.),.UNSPECIFIED.);
#1184=B_SPLINE_CURVE_WITH_KNOTS('',3,(#26567,#26568,#26569,#26570),
 .UNSPECIFIED.,.F.,.F.,(4,4),(-0.082190966342518,0.),.UNSPECIFIED.);
#1185=B_SPLINE_CURVE_WITH_KNOTS('',3,(#26618,#26619,#26620,#26621),
 .UNSPECIFIED.,.F.,.F.,(4,4),(-0.0821972417993147,0.),.UNSPECIFIED.);
#1186=B_SPLINE_CURVE_WITH_KNOTS('',3,(#26629,#26630,#26631,#26632),
 .UNSPECIFIED.,.F.,.F.,(4,4),(-0.0821909663426471,0.),.UNSPECIFIED.);
#1187=B_SPLINE_CURVE_WITH_KNOTS('',3,(#27235,#27236,#27237,#27238,#27239,
#27240,#27241,#27242,#27243,#27244,#27245,#27246,#27247,#27248,#27249,#27250),
 .UNSPECIFIED.,.F.,.F.,(4,3,3,3,3,4),(-4.0925417488383,-3.99994453210988,
-3.49995146559614,-2.99995839908241,-2.49996533256868,-2.0698041887861),
 .UNSPECIFIED.);
#1188=B_SPLINE_CURVE_WITH_KNOTS('',3,(#27253,#27254,#27255,#27256,#27257,
#27258,#27259,#27260,#27261,#27262),.UNSPECIFIED.,.F.,.F.,(4,3,3,4),(0.,
0.499993066513738,0.999986133027476,1.1188550935379),.UNSPECIFIED.);
#1189=B_SPLINE_CURVE_WITH_KNOTS('',3,(#27267,#27268,#27269,#27270,#27271,
#27272,#27273,#27274,#27275,#27276,#27277,#27278,#27279,#27280,#27281,#27282,
#27283,#27284,#27285,#27286,#27287,#27288,#27289,#27290,#27291,#27292,#27293,
#27294,#27295,#27296,#27297,#27298,#27299,#27300,#27301,#27302,#27303,#27304,
#27305,#27306),.UNSPECIFIED.,.F.,.F.,(4,3,3,3,3,3,3,3,3,3,3,3,3,4),(-10.3757270560179,
-9.9998613302747,-9.49986826376097,-8.99987519724723,-8.4998821307335,-7.99988906421976,
-7.49989599770603,-6.99990293119229,-6.49990986467856,-5.99991679816482,
-5.49992373165109,-4.99993066513735,-4.49993759862362,-4.0925417488383),
 .UNSPECIFIED.);
#1190=B_SPLINE_CURVE_WITH_KNOTS('',3,(#27307,#27308,#27309,#27310,#27311,
#27312,#27313,#27314,#27315,#27316,#27317,#27318,#27319,#27320,#27321,#27322,
#27323,#27324,#27325,#27326,#27327,#27328,#27329,#27330,#27331,#27332,#27333,
#27334,#27335,#27336,#27337,#27338,#27339,#27340,#27341,#27342,#27343,#27344,
#27345,#27346),.UNSPECIFIED.,.F.,.F.,(4,3,3,3,3,3,3,3,3,3,3,3,3,4),(1.1188550935379,
1.49997919954121,1.99997226605495,2.49996533256868,2.99995839908241,3.49995146559615,
3.99994453210988,4.49993759862362,4.99993066513735,5.49992373165109,5.99991679816482,
6.49990986467855,6.99990293119229,7.40204040071747),.UNSPECIFIED.);
#1191=B_SPLINE_CURVE_WITH_KNOTS('',3,(#27351,#27352,#27353,#27354,#27355,
#27356,#27357,#27358,#27359,#27360,#27361,#27362,#27363,#27364,#27365,#27366,
#27367,#27368,#27369,#27370,#27371,#27372,#27373,#27374,#27375,#27376,#27377,
#27378,#27379,#27380,#27381,#27382,#27383,#27384,#27385,#27386,#27387,#27388,
#27389,#27390,#27391,#27392,#27393),.UNSPECIFIED.,.F.,.F.,(4,3,3,3,3,3,
3,3,3,3,3,3,3,3,4),(-16.6589123631975,-16.4997711949533,-15.9997781284395,
-15.4997850619258,-14.9997919954121,-14.4997989288983,-13.9998058623846,
-13.4998127958708,-12.9998197293571,-12.4998266628434,-11.9998335963296,
-11.4998405298159,-10.9998474633022,-10.4998543967884,-10.3757270560179),
 .UNSPECIFIED.);
#1192=B_SPLINE_CURVE_WITH_KNOTS('',3,(#27394,#27395,#27396,#27397,#27398,
#27399,#27400,#27401,#27402,#27403,#27404,#27405,#27406,#27407,#27408,#27409,
#27410,#27411,#27412,#27413,#27414,#27415,#27416,#27417,#27418,#27419,#27420,
#27421,#27422,#27423,#27424,#27425,#27426,#27427,#27428,#27429,#27430,#27431,
#27432,#27433,#27434,#27435,#27436),.UNSPECIFIED.,.F.,.F.,(4,3,3,3,3,3,
3,3,3,3,3,3,3,3,4),(7.40204040071747,7.49989599770603,7.99988906421976,
8.4998821307335,8.99987519724724,9.49986826376097,9.99986133027471,10.4998543967884,
10.9998474633022,11.4998405298159,11.9998335963297,12.4998266628434,12.9998197293571,
13.4998127958709,13.6852257078971),.UNSPECIFIED.);
#1193=B_SPLINE_CURVE_WITH_KNOTS('',3,(#27441,#27442,#27443,#27444,#27445,
#27446,#27447,#27448,#27449,#27450,#27451,#27452,#27453,#27454,#27455,#27456,
#27457,#27458,#27459,#27460,#27461,#27462,#27463,#27464,#27465,#27466,#27467,
#27468,#27469,#27470,#27471,#27472,#27473,#27474,#27475,#27476,#27477,#27478,
#27479,#27480),.UNSPECIFIED.,.F.,.F.,(4,3,3,3,3,3,3,3,3,3,3,3,3,4),(-22.942097670377,
-22.4996879931181,-21.9996949266043,-21.4997018600906,-20.9997087935769,
-20.4997157270631,-19.9997226605494,-19.4997295940357,-18.9997365275219,
-18.4997434610082,-17.9997503944945,-17.4997573279807,-16.999764261467,
-16.6589123631975),.UNSPECIFIED.);
#1194=B_SPLINE_CURVE_WITH_KNOTS('',3,(#27481,#27482,#27483,#27484,#27485,
#27486,#27487,#27488,#27489,#27490,#27491,#27492,#27493,#27494,#27495,#27496,
#27497,#27498,#27499,#27500,#27501,#27502,#27503,#27504,#27505,#27506,#27507,
#27508,#27509,#27510,#27511,#27512,#27513,#27514,#27515,#27516,#27517,#27518,
#27519,#27520),.UNSPECIFIED.,.F.,.F.,(4,3,3,3,3,3,3,3,3,3,3,3,3,4),(13.6852257078971,
13.9998058623846,14.4997989288983,14.9997919954121,15.4997850619258,15.9997781284395,
16.4997711949533,16.999764261467,17.4997573279807,17.9997503944945,18.4997434610082,
18.9997365275219,19.4997295940357,19.9684110150766),.UNSPECIFIED.);
#1195=B_SPLINE_CURVE_WITH_KNOTS('',3,(#27525,#27526,#27527,#27528,#27529,
#27530,#27531,#27532,#27533,#27534,#27535,#27536,#27537,#27538,#27539,#27540,
#27541,#27542,#27543,#27544,#27545,#27546,#27547,#27548,#27549,#27550,#27551,
#27552,#27553,#27554,#27555,#27556,#27557,#27558,#27559,#27560,#27561,#27562,
#27563,#27564,#27565,#27566,#27567),.UNSPECIFIED.,.F.,.F.,(4,3,3,3,3,3,
3,3,3,3,3,3,3,3,4),(-29.2252829775567,-28.9995978577966,-28.4996047912829,
-27.9996117247692,-27.4996186582554,-26.9996255917417,-26.499632525228,
-25.9996394587142,-25.4996463922005,-24.9996533256868,-24.499660259173,
-23.9996671926593,-23.4996741261456,-22.9996810596318,-22.942097670377),
 .UNSPECIFIED.);
#1196=B_SPLINE_CURVE_WITH_KNOTS('',3,(#27568,#27569,#27570,#27571,#27572,
#27573,#27574,#27575,#27576,#27577,#27578,#27579,#27580,#27581,#27582,#27583,
#27584,#27585,#27586,#27587,#27588,#27589,#27590,#27591,#27592,#27593,#27594,
#27595,#27596,#27597,#27598,#27599,#27600,#27601,#27602,#27603,#27604,#27605,
#27606,#27607,#27608,#27609,#27610),.UNSPECIFIED.,.F.,.F.,(4,3,3,3,3,3,
3,3,3,3,3,3,3,3,4),(19.9684110150766,19.9997226605494,20.4997157270631,
20.9997087935769,21.4997018600906,21.9996949266044,22.4996879931181,22.9996810596318,
23.4996741261456,23.9996671926593,24.499660259173,24.9996533256868,25.4996463922005,
25.9996394587143,26.2515963222562),.UNSPECIFIED.);
#1197=B_SPLINE_CURVE_WITH_KNOTS('',3,(#27615,#27616,#27617,#27618,#27619,
#27620,#27621,#27622,#27623,#27624,#27625,#27626,#27627,#27628,#27629,#27630,
#27631,#27632,#27633,#27634,#27635,#27636,#27637,#27638,#27639,#27640,#27641,
#27642,#27643,#27644,#27645,#27646,#27647,#27648,#27649,#27650,#27651,#27652,
#27653,#27654,#27655,#27656,#27657),.UNSPECIFIED.,.F.,.F.,(4,3,3,3,3,3,
3,3,3,3,3,3,3,3,4),(-35.5084682847362,-35.4995077224752,-34.9995146559615,
-34.4995215894477,-33.999528522934,-33.4995354564203,-32.9995423899065,
-32.4995493233928,-31.9995562568791,-31.4995631903653,-30.9995701238516,
-30.4995770573379,-29.9995839908241,-29.4995909243104,-29.2252829775567),
 .UNSPECIFIED.);
#1198=B_SPLINE_CURVE_WITH_KNOTS('',3,(#27658,#27659,#27660,#27661,#27662,
#27663,#27664,#27665,#27666,#27667,#27668,#27669,#27670,#27671,#27672,#27673,
#27674,#27675,#27676,#27677,#27678,#27679,#27680,#27681,#27682,#27683,#27684,
#27685,#27686,#27687,#27688,#27689,#27690,#27691,#27692,#27693,#27694,#27695,
#27696,#27697,#27698,#27699,#27700),.UNSPECIFIED.,.F.,.F.,(4,3,3,3,3,3,
3,3,3,3,3,3,3,3,4),(26.2515963222562,26.499632525228,26.9996255917417,27.4996186582555,
27.9996117247692,28.4996047912829,28.9995978577967,29.4995909243104,29.9995839908241,
30.4995770573378,30.9995701238516,31.4995631903653,31.999556256879,32.4995493233928,
32.5347816294358),.UNSPECIFIED.);
#1199=B_SPLINE_CURVE_WITH_KNOTS('',3,(#27705,#27706,#27707,#27708,#27709,
#27710,#27711,#27712,#27713,#27714,#27715,#27716,#27717,#27718,#27719,#27720,
#27721,#27722,#27723,#27724,#27725,#27726,#27727,#27728,#27729,#27730,#27731,
#27732,#27733,#27734,#27735,#27736,#27737,#27738,#27739,#27740,#27741,#27742,
#27743,#27744),.UNSPECIFIED.,.F.,.F.,(4,3,3,3,3,3,3,3,3,3,3,3,3,4),(-41.7916535919158,
-41.49942452064,-40.9994314541263,-40.4994383876125,-39.9994453210988,-39.4994522545851,
-38.9994591880713,-38.4994661215576,-37.9994730550439,-37.4994799885301,
-36.9994869220164,-36.4994938555027,-35.9995007889889,-35.5084682847362),
 .UNSPECIFIED.);
#1200=B_SPLINE_CURVE_WITH_KNOTS('',3,(#27745,#27746,#27747,#27748,#27749,
#27750,#27751,#27752,#27753,#27754,#27755,#27756,#27757,#27758,#27759,#27760,
#27761,#27762,#27763,#27764,#27765,#27766,#27767,#27768,#27769,#27770,#27771,
#27772,#27773,#27774,#27775,#27776,#27777,#27778,#27779,#27780,#27781,#27782,
#27783,#27784),.UNSPECIFIED.,.F.,.F.,(4,3,3,3,3,3,3,3,3,3,3,3,3,4),(32.5347816294358,
32.9995423899065,33.4995354564203,33.999528522934,34.4995215894477,34.9995146559615,
35.4995077224752,35.999500788989,36.4994938555027,36.9994869220164,37.4994799885302,
37.9994730550439,38.4994661215576,38.8179669366154),.UNSPECIFIED.);
#1201=B_SPLINE_CURVE_WITH_KNOTS('',3,(#27789,#27790,#27791,#27792,#27793,
#27794,#27795,#27796,#27797,#27798,#27799,#27800,#27801,#27802,#27803,#27804,
#27805,#27806,#27807,#27808,#27809,#27810,#27811,#27812,#27813,#27814,#27815,
#27816,#27817,#27818,#27819,#27820,#27821,#27822,#27823,#27824,#27825,#27826,
#27827,#27828,#27829,#27830,#27831),.UNSPECIFIED.,.F.,.F.,(4,3,3,3,3,3,
3,3,3,3,3,3,3,3,4),(-48.0748388990954,-47.9993343853186,-47.4993413188049,
-46.9993482522911,-46.4993551857774,-45.9993621192636,-45.4993690527499,
-44.9993759862362,-44.4993829197224,-43.9993898532087,-43.499396786695,
-42.9994037201812,-42.4994106536675,-41.9994175871538,-41.7916535919158),
 .UNSPECIFIED.);
#1202=B_SPLINE_CURVE_WITH_KNOTS('',3,(#27832,#27833,#27834,#27835,#27836,
#27837,#27838,#27839,#27840,#27841,#27842,#27843,#27844,#27845,#27846,#27847,
#27848,#27849,#27850,#27851,#27852,#27853,#27854,#27855,#27856,#27857,#27858,
#27859,#27860,#27861,#27862,#27863,#27864,#27865,#27866,#27867,#27868,#27869,
#27870,#27871,#27872,#27873,#27874),.UNSPECIFIED.,.F.,.F.,(4,3,3,3,3,3,
3,3,3,3,3,3,3,3,4),(38.8179669366154,38.9994591880714,39.4994522545851,
39.9994453210988,40.4994383876126,40.9994314541263,41.49942452064,41.9994175871538,
42.4994106536675,42.9994037201812,43.499396786695,43.9993898532087,44.4993829197224,
44.9993759862362,45.101152243795),.UNSPECIFIED.);
#1203=B_SPLINE_CURVE_WITH_KNOTS('',3,(#27879,#27880,#27881,#27882,#27883,
#27884,#27885,#27886,#27887,#27888,#27889,#27890,#27891,#27892,#27893,#27894,
#27895,#27896,#27897,#27898,#27899,#27900,#27901,#27902,#27903,#27904,#27905,
#27906,#27907,#27908,#27909,#27910,#27911,#27912,#27913,#27914,#27915,#27916,
#27917,#27918),.UNSPECIFIED.,.F.,.F.,(4,3,3,3,3,3,3,3,3,3,3,3,3,4),(-54.358024206275,
-53.9992511834834,-53.4992581169697,-52.9992650504559,-52.4992719839422,
-51.9992789174285,-51.4992858509147,-50.999292784401,-50.4992997178873,
-49.9993066513735,-49.4993135848598,-48.999320518346,-48.4993274518323,
-48.0748388990954),.UNSPECIFIED.);
#1204=B_SPLINE_CURVE_WITH_KNOTS('',3,(#27919,#27920,#27921,#27922,#27923,
#27924,#27925,#27926,#27927,#27928,#27929,#27930,#27931,#27932,#27933,#27934,
#27935,#27936,#27937,#27938,#27939,#27940,#27941,#27942,#27943,#27944,#27945,
#27946,#27947,#27948,#27949,#27950,#27951,#27952,#27953,#27954,#27955,#27956,
#27957,#27958),.UNSPECIFIED.,.F.,.F.,(4,3,3,3,3,3,3,3,3,3,3,3,3,4),(45.101152243795,
45.4993690527499,45.9993621192636,46.4993551857774,46.9993482522911,47.4993413188049,
47.9993343853186,48.4993274518323,48.9993205183461,49.4993135848598,49.9993066513735,
50.4992997178873,50.999292784401,51.3843375509746),.UNSPECIFIED.);
#1205=B_SPLINE_CURVE_WITH_KNOTS('',3,(#27963,#27964,#27965,#27966,#27967,
#27968,#27969,#27970,#27971,#27972,#27973,#27974,#27975,#27976,#27977,#27978,
#27979,#27980,#27981,#27982,#27983,#27984,#27985,#27986,#27987,#27988,#27989,
#27990,#27991,#27992,#27993,#27994,#27995,#27996,#27997,#27998,#27999,#28000,
#28001,#28002,#28003,#28004,#28005),.UNSPECIFIED.,.F.,.F.,(4,3,3,3,3,3,
3,3,3,3,3,3,3,3,4),(-60.6412095134546,-60.499161048162,-59.9991679816482,
-59.4991749151345,-58.9991818486208,-58.499188782107,-57.9991957155933,
-57.4992026490795,-56.9992095825658,-56.4992165160521,-55.9992234495383,
-55.4992303830246,-54.9992373165109,-54.4992442499971,-54.358024206275),
 .UNSPECIFIED.);
#1206=B_SPLINE_CURVE_WITH_KNOTS('',3,(#28006,#28007,#28008,#28009,#28010,
#28011,#28012,#28013,#28014,#28015,#28016,#28017,#28018,#28019,#28020,#28021,
#28022,#28023,#28024,#28025,#28026,#28027,#28028,#28029,#28030,#28031,#28032,
#28033,#28034,#28035,#28036,#28037,#28038,#28039,#28040,#28041,#28042,#28043,
#28044,#28045,#28046,#28047,#28048),.UNSPECIFIED.,.F.,.F.,(4,3,3,3,3,3,
3,3,3,3,3,3,3,3,4),(51.3843375509746,51.4992858509148,51.9992789174285,
52.4992719839422,52.999265050456,53.4992581169697,53.9992511834834,54.4992442499972,
54.9992373165109,55.4992303830246,55.9992234495384,56.4992165160521,56.9992095825658,
57.4992026490796,57.6675228581542),.UNSPECIFIED.);
#1207=B_SPLINE_CURVE_WITH_KNOTS('',3,(#28053,#28054,#28055,#28056,#28057,
#28058,#28059,#28060,#28061,#28062,#28063,#28064,#28065,#28066,#28067,#28068,
#28069,#28070,#28071,#28072,#28073,#28074,#28075,#28076,#28077,#28078,#28079,
#28080,#28081,#28082,#28083,#28084,#28085,#28086,#28087,#28088,#28089,#28090,
#28091,#28092),.UNSPECIFIED.,.F.,.F.,(4,3,3,3,3,3,3,3,3,3,3,3,3,4),(-66.9243948206342,
-66.4990778463268,-65.999084779813,-65.4990917132993,-64.9990986467856,
-64.4991055802718,-63.9991125137581,-63.4991194472444,-62.9991263807306,
-62.4991333142169,-61.9991402477032,-61.4991471811894,-60.9991541146757,
-60.6412095134546),.UNSPECIFIED.);
#1208=B_SPLINE_CURVE_WITH_KNOTS('',3,(#28093,#28094,#28095,#28096,#28097,
#28098,#28099,#28100,#28101,#28102,#28103,#28104,#28105,#28106,#28107,#28108,
#28109,#28110,#28111,#28112,#28113,#28114,#28115,#28116,#28117,#28118,#28119,
#28120,#28121,#28122,#28123,#28124,#28125,#28126,#28127,#28128,#28129,#28130,
#28131,#28132),.UNSPECIFIED.,.F.,.F.,(4,3,3,3,3,3,3,3,3,3,3,3,3,4),(57.6675228581542,
57.9991957155933,58.499188782107,58.9991818486208,59.4991749151345,59.9991679816482,
60.499161048162,60.9991541146757,61.4991471811894,61.9991402477032,62.4991333142169,
62.9991263807307,63.4991194472444,63.9507081653338),.UNSPECIFIED.);
#1209=B_SPLINE_CURVE_WITH_KNOTS('',3,(#28137,#28138,#28139,#28140,#28141,
#28142,#28143,#28144,#28145,#28146,#28147,#28148,#28149,#28150,#28151,#28152,
#28153,#28154,#28155,#28156,#28157,#28158,#28159,#28160,#28161,#28162,#28163,
#28164,#28165,#28166,#28167,#28168,#28169,#28170,#28171,#28172,#28173,#28174,
#28175,#28176,#28177,#28178,#28179),.UNSPECIFIED.,.F.,.F.,(4,3,3,3,3,3,
3,3,3,3,3,3,3,3,4),(-73.2075801278138,-72.9989877110053,-72.4989946444916,
-71.9990015779779,-71.4990085114641,-70.9990154449504,-70.4990223784367,
-69.9990293119229,-69.4990362454092,-68.9990431788954,-68.4990501123817,
-67.999057045868,-67.4990639793542,-66.9990709128405,-66.9243948206342),
 .UNSPECIFIED.);
#1210=B_SPLINE_CURVE_WITH_KNOTS('',3,(#28180,#28181,#28182,#28183,#28184,
#28185,#28186,#28187,#28188,#28189,#28190,#28191,#28192,#28193,#28194,#28195,
#28196,#28197,#28198,#28199,#28200,#28201,#28202,#28203,#28204,#28205,#28206,
#28207,#28208,#28209,#28210,#28211,#28212,#28213,#28214,#28215,#28216,#28217,
#28218,#28219,#28220,#28221,#28222),.UNSPECIFIED.,.F.,.F.,(4,3,3,3,3,3,
3,3,3,3,3,3,3,3,4),(63.9507081653338,63.9991125137581,64.4991055802719,
64.9990986467856,65.4990917132993,65.9990847798131,66.4990778463268,66.9990709128405,
67.4990639793543,67.999057045868,68.4990501123817,68.9990431788954,69.4990362454092,
69.9990293119229,70.2338934725134),.UNSPECIFIED.);
#1211=B_SPLINE_CURVE_WITH_KNOTS('',3,(#28227,#28228,#28229,#28230,#28231,
#28232,#28233,#28234,#28235,#28236,#28237,#28238,#28239,#28240,#28241,#28242,
#28243,#28244,#28245,#28246,#28247,#28248,#28249,#28250,#28251,#28252,#28253,
#28254,#28255,#28256,#28257,#28258,#28259,#28260,#28261,#28262,#28263,#28264,
#28265,#28266),.UNSPECIFIED.,.F.,.F.,(4,3,3,3,3,3,3,3,3,3,3,3,3,4),(-79.4907654349934,
-78.9989045091702,-78.4989114426564,-77.9989183761427,-77.498925309629,
-76.9989322431152,-76.4989391766015,-75.9989461100877,-75.498953043574,
-74.9989599770603,-74.4989669105465,-73.9989738440328,-73.4989807775191,
-73.2075801278138),.UNSPECIFIED.);
#1212=B_SPLINE_CURVE_WITH_KNOTS('',3,(#28267,#28268,#28269,#28270,#28271,
#28272,#28273,#28274,#28275,#28276,#28277,#28278,#28279,#28280,#28281,#28282,
#28283,#28284,#28285,#28286,#28287,#28288,#28289,#28290,#28291,#28292,#28293,
#28294,#28295,#28296,#28297,#28298,#28299,#28300,#28301,#28302,#28303,#28304,
#28305,#28306,#28307,#28308,#28309),.UNSPECIFIED.,.F.,.F.,(4,3,3,3,3,3,
3,3,3,3,3,3,3,3,4),(70.2338934725134,70.4990223784366,70.9990154449504,
71.4990085114641,71.9990015779779,72.4989946444916,72.9989877110053,73.4989807775191,
73.9989738440328,74.4989669105466,74.9989599770603,75.498953043574,75.9989461100878,
76.4989391766015,76.517078779693),.UNSPECIFIED.);
#1213=B_SPLINE_CURVE_WITH_KNOTS('',3,(#28314,#28315,#28316,#28317,#28318,
#28319,#28320,#28321,#28322,#28323,#28324,#28325,#28326,#28327,#28328,#28329,
#28330,#28331,#28332,#28333,#28334,#28335,#28336,#28337,#28338,#28339,#28340,
#28341,#28342,#28343,#28344,#28345,#28346,#28347,#28348,#28349,#28350,#28351,
#28352,#28353,#28354,#28355,#28356),.UNSPECIFIED.,.F.,.F.,(4,3,3,3,3,3,
3,3,3,3,3,3,3,3,4),(-85.773950742173,-85.4988143738487,-84.998821307335,
-84.4988282408213,-83.9988351743075,-83.4988421077938,-82.9988490412801,
-82.4988559747663,-81.9988629082526,-81.4988698417388,-80.9988767752251,
-80.4988837087114,-79.9988906421976,-79.4988975756839,-79.4907654349934),
 .UNSPECIFIED.);
#1214=B_SPLINE_CURVE_WITH_KNOTS('',3,(#28357,#28358,#28359,#28360,#28361,
#28362,#28363,#28364,#28365,#28366,#28367,#28368,#28369,#28370,#28371,#28372,
#28373,#28374,#28375,#28376,#28377,#28378,#28379,#28380,#28381,#28382,#28383,
#28384,#28385,#28386,#28387,#28388,#28389,#28390,#28391,#28392,#28393,#28394,
#28395,#28396),.UNSPECIFIED.,.F.,.F.,(4,3,3,3,3,3,3,3,3,3,3,3,3,4),(76.517078779693,
76.9989322431153,77.498925309629,77.9989183761427,78.4989114426564,78.9989045091702,
79.4988975756839,79.9988906421977,80.4988837087114,80.9988767752251,81.4988698417389,
81.9988629082526,82.4988559747663,82.8002640868726),.UNSPECIFIED.);
#1215=B_SPLINE_CURVE_WITH_KNOTS('',3,(#28401,#28402,#28403,#28404,#28405,
#28406,#28407,#28408,#28409,#28410,#28411,#28412,#28413,#28414,#28415,#28416,
#28417,#28418,#28419,#28420,#28421,#28422,#28423,#28424,#28425,#28426,#28427,
#28428,#28429,#28430,#28431,#28432,#28433,#28434,#28435,#28436,#28437,#28438,
#28439,#28440,#28441,#28442,#28443),.UNSPECIFIED.,.F.,.F.,(4,3,3,3,3,3,
3,3,3,3,3,3,3,3,4),(-92.0571360493526,-91.9987242385273,-91.4987311720135,
-90.9987381054998,-90.4987450389861,-89.9987519724723,-89.4987589059586,
-88.9987658394449,-88.4987727729311,-87.9987797064174,-87.4987866399037,
-86.9987935733899,-86.4988005068762,-85.9988074403625,-85.773950742173),
 .UNSPECIFIED.);
#1216=B_SPLINE_CURVE_WITH_KNOTS('',3,(#28444,#28445,#28446,#28447,#28448,
#28449,#28450,#28451,#28452,#28453,#28454,#28455,#28456,#28457,#28458,#28459,
#28460,#28461,#28462,#28463,#28464,#28465,#28466,#28467,#28468,#28469,#28470,
#28471,#28472,#28473,#28474,#28475,#28476,#28477,#28478,#28479,#28480,#28481,
#28482,#28483,#28484,#28485,#28486),.UNSPECIFIED.,.F.,.F.,(4,3,3,3,3,3,
3,3,3,3,3,3,3,3,4),(82.8002640868726,82.9988490412801,83.4988421077938,
83.9988351743075,84.4988282408213,84.998821307335,85.4988143738488,85.9988074403625,
86.4988005068762,86.99879357339,87.4987866399037,87.9987797064175,88.4987727729312,
88.9987658394449,89.0834493940522),.UNSPECIFIED.);
#1217=B_SPLINE_CURVE_WITH_KNOTS('',3,(#28491,#28492,#28493,#28494,#28495,
#28496,#28497,#28498,#28499,#28500,#28501,#28502,#28503,#28504,#28505,#28506,
#28507,#28508,#28509,#28510,#28511,#28512,#28513,#28514,#28515,#28516,#28517,
#28518,#28519,#28520,#28521,#28522,#28523,#28524,#28525,#28526,#28527,#28528,
#28529,#28530),.UNSPECIFIED.,.F.,.F.,(4,3,3,3,3,3,3,3,3,3,3,3,3,4),(-98.3403213565321,
-97.9986410366921,-97.4986479701784,-96.9986549036646,-96.4986618371509,
-95.9986687706372,-95.4986757041234,-94.9986826376097,-94.4986895710959,
-93.9986965045822,-93.4987034380685,-92.9987103715547,-92.498717305041,
-92.0571360493526),.UNSPECIFIED.);
#1218=B_SPLINE_CURVE_WITH_KNOTS('',3,(#28531,#28532,#28533,#28534,#28535,
#28536,#28537,#28538,#28539,#28540,#28541,#28542,#28543,#28544,#28545,#28546,
#28547,#28548,#28549,#28550,#28551,#28552,#28553,#28554,#28555,#28556,#28557,
#28558,#28559,#28560,#28561,#28562,#28563,#28564,#28565,#28566,#28567,#28568,
#28569,#28570),.UNSPECIFIED.,.F.,.F.,(4,3,3,3,3,3,3,3,3,3,3,3,3,4),(89.0834493940522,
89.4987589059587,89.9987519724724,90.4987450389861,90.9987381054998,91.4987311720136,
91.9987242385273,92.498717305041,92.9987103715548,93.4987034380685,93.9986965045822,
94.498689571096,94.9986826376097,95.3666347012317),.UNSPECIFIED.);
#1219=B_SPLINE_CURVE_WITH_KNOTS('',3,(#28575,#28576,#28577,#28578,#28579,
#28580,#28581,#28582,#28583,#28584,#28585,#28586,#28587,#28588,#28589,#28590,
#28591,#28592,#28593,#28594,#28595,#28596,#28597,#28598,#28599,#28600,#28601,
#28602,#28603,#28604,#28605,#28606,#28607,#28608,#28609,#28610,#28611,#28612,
#28613,#28614,#28615,#28616,#28617),.UNSPECIFIED.,.F.,.F.,(4,3,3,3,3,3,
3,3,3,3,3,3,3,3,4),(-104.623506663712,-104.498550901371,-103.998557834857,
-103.498564768343,-102.998571701829,-102.498578635316,-101.998585568802,
-101.498592502288,-100.998599435775,-100.498606369261,-99.998613302747,
-99.4986202362333,-98.9986271697196,-98.4986341032058,-98.3403213565321),
 .UNSPECIFIED.);
#1220=B_SPLINE_CURVE_WITH_KNOTS('',3,(#28618,#28619,#28620,#28621,#28622,
#28623,#28624,#28625,#28626,#28627,#28628,#28629,#28630,#28631,#28632,#28633,
#28634,#28635,#28636,#28637,#28638,#28639,#28640,#28641,#28642,#28643,#28644,
#28645,#28646,#28647,#28648,#28649,#28650,#28651,#28652,#28653,#28654,#28655,
#28656,#28657,#28658,#28659,#28660),.UNSPECIFIED.,.F.,.F.,(4,3,3,3,3,3,
3,3,3,3,3,3,3,3,4),(95.3666347012317,95.4986757041234,95.9986687706372,
96.4986618371509,96.9986549036646,97.4986479701784,97.9986410366921,98.4986341032058,
98.9986271697196,99.4986202362333,99.9986133027471,100.498606369261,100.998599435775,
101.498592502288,101.649820008411),.UNSPECIFIED.);
#1221=B_SPLINE_CURVE_WITH_KNOTS('',3,(#28665,#28666,#28667,#28668,#28669,
#28670,#28671,#28672,#28673,#28674,#28675,#28676,#28677,#28678,#28679,#28680,
#28681,#28682,#28683,#28684,#28685,#28686,#28687,#28688,#28689,#28690,#28691,
#28692,#28693,#28694,#28695,#28696,#28697,#28698,#28699,#28700,#28701,#28702,
#28703,#28704),.UNSPECIFIED.,.F.,.F.,(4,3,3,3,3,3,3,3,3,3,3,3,3,4),(-110.906691970891,
-110.498467699535,-109.998474633022,-109.498481566508,-108.998488499994,
-108.498495433481,-107.998502366967,-107.498509300453,-106.998516233939,
-106.498523167426,-105.998530100912,-105.498537034398,-104.998543967884,
-104.623506663712),.UNSPECIFIED.);
#1222=B_SPLINE_CURVE_WITH_KNOTS('',3,(#28705,#28706,#28707,#28708,#28709,
#28710,#28711,#28712,#28713,#28714,#28715,#28716,#28717,#28718,#28719,#28720,
#28721,#28722,#28723,#28724,#28725,#28726,#28727,#28728,#28729,#28730,#28731,
#28732,#28733,#28734,#28735,#28736,#28737,#28738,#28739,#28740,#28741,#28742,
#28743,#28744),.UNSPECIFIED.,.F.,.F.,(4,3,3,3,3,3,3,3,3,3,3,3,3,4),(101.649820008411,
101.998585568802,102.498578635316,102.998571701829,103.498564768343,103.998557834857,
104.498550901371,104.998543967884,105.498537034398,105.998530100912,106.498523167426,
106.998516233939,107.498509300453,107.933005315591),.UNSPECIFIED.);
#1223=B_SPLINE_CURVE_WITH_KNOTS('',3,(#28749,#28750,#28751,#28752,#28753,
#28754,#28755,#28756,#28757,#28758,#28759,#28760,#28761,#28762,#28763,#28764,
#28765,#28766,#28767,#28768,#28769,#28770,#28771,#28772,#28773,#28774,#28775,
#28776,#28777,#28778,#28779,#28780,#28781,#28782,#28783,#28784,#28785,#28786,
#28787,#28788,#28789,#28790,#28791),.UNSPECIFIED.,.F.,.F.,(4,3,3,3,3,3,
3,3,3,3,3,3,3,3,4),(-117.189877278071,-116.998377564214,-116.4983844977,
-115.998391431187,-115.498398364673,-114.998405298159,-114.498412231645,
-113.998419165132,-113.498426098618,-112.998433032104,-112.49843996559,
-111.998446899077,-111.498453832563,-110.998460766049,-110.906691970891),
 .UNSPECIFIED.);
#1224=B_SPLINE_CURVE_WITH_KNOTS('',3,(#28792,#28793,#28794,#28795,#28796,
#28797,#28798,#28799,#28800,#28801,#28802,#28803,#28804,#28805,#28806,#28807,
#28808,#28809,#28810,#28811,#28812,#28813,#28814,#28815,#28816,#28817,#28818,
#28819,#28820,#28821,#28822,#28823,#28824,#28825,#28826,#28827,#28828,#28829,
#28830,#28831,#28832,#28833,#28834),.UNSPECIFIED.,.F.,.F.,(4,3,3,3,3,3,
3,3,3,3,3,3,3,3,4),(107.933005315591,107.998502366967,108.498495433481,
108.998488499994,109.498481566508,109.998474633022,110.498467699536,110.998460766049,
111.498453832563,111.998446899077,112.49843996559,112.998433032104,113.498426098618,
113.998419165132,114.216190622771),.UNSPECIFIED.);
#1225=B_SPLINE_CURVE_WITH_KNOTS('',3,(#28839,#28840,#28841,#28842,#28843,
#28844,#28845,#28846,#28847,#28848,#28849,#28850,#28851,#28852,#28853,#28854,
#28855,#28856,#28857,#28858,#28859,#28860,#28861,#28862,#28863,#28864,#28865,
#28866,#28867,#28868,#28869,#28870,#28871,#28872,#28873,#28874,#28875,#28876,
#28877,#28878),.UNSPECIFIED.,.F.,.F.,(4,3,3,3,3,3,3,3,3,3,3,3,3,4),(-123.473062585251,
-122.998294362379,-122.498301295865,-121.998308229351,-121.498315162838,
-120.998322096324,-120.49832902981,-119.998335963296,-119.498342896783,
-118.998349830269,-118.498356763755,-117.998363697241,-117.498370630728,
-117.189877278071),.UNSPECIFIED.);
#1226=B_SPLINE_CURVE_WITH_KNOTS('',3,(#28879,#28880,#28881,#28882,#28883,
#28884,#28885,#28886,#28887,#28888,#28889,#28890,#28891,#28892,#28893,#28894,
#28895,#28896,#28897,#28898,#28899,#28900,#28901,#28902,#28903,#28904,#28905,
#28906,#28907,#28908,#28909,#28910,#28911,#28912,#28913,#28914,#28915,#28916,
#28917,#28918),.UNSPECIFIED.,.F.,.F.,(4,3,3,3,3,3,3,3,3,3,3,3,3,4),(114.216190622771,
114.498412231645,114.998405298159,115.498398364673,115.998391431187,116.4983844977,
116.998377564214,117.498370630728,117.998363697242,118.498356763755,118.998349830269,
119.498342896783,119.998335963296,120.49937592995),.UNSPECIFIED.);
#1227=B_SPLINE_CURVE_WITH_KNOTS('',3,(#28923,#28924,#28925,#28926,#28927,
#28928,#28929,#28930,#28931,#28932,#28933,#28934,#28935,#28936,#28937,#28938,
#28939,#28940,#28941,#28942,#28943,#28944,#28945,#28946,#28947,#28948,#28949,
#28950,#28951,#28952,#28953,#28954,#28955,#28956,#28957,#28958,#28959,#28960,
#28961,#28962,#28963,#28964,#28965),.UNSPECIFIED.,.F.,.F.,(4,3,3,3,3,3,
3,3,3,3,3,3,3,3,4),(-129.75624789243,-129.498204227057,-128.998211160544,
-128.49821809403,-127.998225027516,-127.498231961002,-126.998238894489,
-126.498245827975,-125.998252761461,-125.498259694948,-124.998266628434,
-124.49827356192,-123.998280495406,-123.498287428893,-123.473062585251),
 .UNSPECIFIED.);
#1228=B_SPLINE_CURVE_WITH_KNOTS('',3,(#28966,#28967,#28968,#28969,#28970,
#28971,#28972,#28973,#28974,#28975,#28976,#28977,#28978,#28979,#28980,#28981,
#28982,#28983,#28984,#28985,#28986,#28987,#28988,#28989,#28990,#28991,#28992,
#28993,#28994,#28995,#28996,#28997,#28998,#28999,#29000,#29001,#29002,#29003,
#29004,#29005),.UNSPECIFIED.,.F.,.F.,(4,3,3,3,3,3,3,3,3,3,3,3,3,4),(120.49937592995,
120.998322096324,121.498315162838,121.998308229351,122.498301295865,122.998294362379,
123.498287428893,123.998280495406,124.49827356192,124.998266628434,125.498259694948,
125.998252761461,126.498245827975,126.78256123713),.UNSPECIFIED.);
#1229=B_SPLINE_CURVE_WITH_KNOTS('',3,(#29010,#29011,#29012,#29013,#29014,
#29015,#29016,#29017,#29018,#29019,#29020,#29021,#29022,#29023,#29024,#29025,
#29026,#29027,#29028,#29029,#29030,#29031,#29032,#29033,#29034,#29035,#29036,
#29037,#29038,#29039,#29040,#29041,#29042,#29043,#29044,#29045,#29046,#29047,
#29048,#29049,#29050,#29051,#29052),.UNSPECIFIED.,.F.,.F.,(4,3,3,3,3,3,
3,3,3,3,3,3,3,3,4),(-136.03943319961,-135.998114091736,-135.498121025222,
-134.998127958708,-134.498134892195,-133.998141825681,-133.498148759167,
-132.998155692654,-132.49816262614,-131.998169559626,-131.498176493112,
-130.998183426599,-130.498190360085,-129.998197293571,-129.75624789243),
 .UNSPECIFIED.);
#1230=B_SPLINE_CURVE_WITH_KNOTS('',3,(#29053,#29054,#29055,#29056,#29057,
#29058,#29059,#29060,#29061,#29062,#29063,#29064,#29065,#29066,#29067,#29068,
#29069,#29070,#29071,#29072,#29073,#29074,#29075,#29076,#29077,#29078,#29079,
#29080,#29081,#29082,#29083,#29084,#29085,#29086,#29087,#29088,#29089,#29090,
#29091,#29092,#29093,#29094,#29095),.UNSPECIFIED.,.F.,.F.,(4,3,3,3,3,3,
3,3,3,3,3,3,3,3,4),(126.78256123713,126.998238894489,127.498231961003,127.998225027516,
128.49821809403,128.998211160544,129.498204227057,129.998197293571,130.498190360085,
130.998183426599,131.498176493112,131.998169559626,132.49816262614,132.998155692654,
133.065746544309),.UNSPECIFIED.);
#1231=B_SPLINE_CURVE_WITH_KNOTS('',3,(#29100,#29101,#29102,#29103,#29104,
#29105,#29106,#29107,#29108,#29109,#29110,#29111,#29112,#29113,#29114,#29115,
#29116,#29117,#29118,#29119,#29120,#29121,#29122,#29123,#29124,#29125,#29126,
#29127,#29128,#29129,#29130,#29131,#29132,#29133,#29134,#29135,#29136,#29137,
#29138,#29139),.UNSPECIFIED.,.F.,.F.,(4,3,3,3,3,3,3,3,3,3,3,3,3,4),(-142.322618506789,
-141.998030889901,-141.498037823387,-140.998044756873,-140.49805169036,
-139.998058623846,-139.498065557332,-138.998072490818,-138.498079424305,
-137.998086357791,-137.498093291277,-136.998100224763,-136.49810715825,
-136.03943319961),.UNSPECIFIED.);
#1232=B_SPLINE_CURVE_WITH_KNOTS('',3,(#29140,#29141,#29142,#29143,#29144,
#29145,#29146,#29147,#29148,#29149,#29150,#29151,#29152,#29153,#29154,#29155,
#29156,#29157,#29158,#29159,#29160,#29161,#29162,#29163,#29164,#29165,#29166,
#29167,#29168,#29169,#29170,#29171,#29172,#29173,#29174,#29175,#29176,#29177,
#29178,#29179),.UNSPECIFIED.,.F.,.F.,(4,3,3,3,3,3,3,3,3,3,3,3,3,4),(133.065746544309,
133.498148759167,133.998141825681,134.498134892195,134.998127958709,135.498121025222,
135.998114091736,136.49810715825,136.998100224763,137.498093291277,137.998086357791,
138.498079424305,138.998072490818,139.348931851489),.UNSPECIFIED.);
#1233=B_SPLINE_CURVE_WITH_KNOTS('',3,(#29184,#29185,#29186,#29187,#29188,
#29189,#29190,#29191,#29192,#29193,#29194,#29195,#29196,#29197,#29198,#29199,
#29200,#29201,#29202,#29203,#29204,#29205,#29206,#29207,#29208,#29209,#29210,
#29211,#29212,#29213,#29214,#29215,#29216,#29217,#29218,#29219,#29220,#29221,
#29222,#29223,#29224,#29225,#29226),.UNSPECIFIED.,.F.,.F.,(4,3,3,3,3,3,
3,3,3,3,3,3,3,3,4),(-148.605803813969,-148.497940754579,-147.997947688066,
-147.497954621552,-146.997961555038,-146.497968488524,-145.997975422011,
-145.497982355497,-144.997989288983,-144.497996222469,-143.998003155956,
-143.498010089442,-142.998017022928,-142.498023956414,-142.322618506789),
 .UNSPECIFIED.);
#1234=B_SPLINE_CURVE_WITH_KNOTS('',3,(#29227,#29228,#29229,#29230,#29231,
#29232,#29233,#29234,#29235,#29236,#29237,#29238,#29239,#29240,#29241,#29242,
#29243,#29244,#29245,#29246,#29247,#29248,#29249,#29250,#29251,#29252,#29253,
#29254,#29255,#29256,#29257,#29258,#29259,#29260,#29261,#29262,#29263,#29264,
#29265,#29266,#29267,#29268,#29269),.UNSPECIFIED.,.F.,.F.,(4,3,3,3,3,3,
3,3,3,3,3,3,3,3,4),(139.348931851489,139.498065557332,139.998058623846,
140.49805169036,140.998044756873,141.498037823387,141.998030889901,142.498023956415,
142.998017022928,143.498010089442,143.998003155956,144.497996222469,144.997989288983,
145.497982355497,145.632117158668),.UNSPECIFIED.);
#1235=B_SPLINE_CURVE_WITH_KNOTS('',3,(#29274,#29275,#29276,#29277,#29278,
#29279,#29280,#29281,#29282,#29283,#29284,#29285,#29286,#29287,#29288,#29289,
#29290,#29291,#29292,#29293,#29294,#29295,#29296,#29297,#29298,#29299,#29300,
#29301,#29302,#29303,#29304,#29305,#29306,#29307,#29308,#29309,#29310,#29311,
#29312,#29313),.UNSPECIFIED.,.F.,.F.,(4,3,3,3,3,3,3,3,3,3,3,3,3,4),(-154.888989121148,
-154.497857552744,-153.99786448623,-153.497871419717,-152.997878353203,
-152.497885286689,-151.997892220175,-151.497899153662,-150.997906087148,
-150.497913020634,-149.997919954121,-149.497926887607,-148.997933821093,
-148.605803813969),.UNSPECIFIED.);
#1236=B_SPLINE_CURVE_WITH_KNOTS('',3,(#29314,#29315,#29316,#29317,#29318,
#29319,#29320,#29321,#29322,#29323,#29324,#29325,#29326,#29327,#29328,#29329,
#29330,#29331,#29332,#29333,#29334,#29335,#29336,#29337,#29338,#29339,#29340,
#29341,#29342,#29343,#29344,#29345,#29346,#29347,#29348,#29349,#29350,#29351,
#29352,#29353),.UNSPECIFIED.,.F.,.F.,(4,3,3,3,3,3,3,3,3,3,3,3,3,4),(145.632117158668,
145.997975422011,146.497968488524,146.997961555038,147.497954621552,147.997947688066,
148.497940754579,148.997933821093,149.497926887607,149.997919954121,150.497913020634,
150.997906087148,151.497899153662,151.915302465848),.UNSPECIFIED.);
#1237=B_SPLINE_CURVE_WITH_KNOTS('',3,(#29358,#29359,#29360,#29361,#29362,
#29363,#29364,#29365,#29366,#29367,#29368,#29369,#29370,#29371,#29372,#29373,
#29374,#29375,#29376,#29377,#29378,#29379,#29380,#29381,#29382,#29383,#29384,
#29385,#29386,#29387,#29388,#29389,#29390,#29391,#29392,#29393,#29394,#29395,
#29396,#29397,#29398,#29399,#29400),.UNSPECIFIED.,.F.,.F.,(4,3,3,3,3,3,
3,3,3,3,3,3,3,3,4),(-161.172174428328,-160.997767417423,-160.497774350909,
-159.997781284395,-159.497788217882,-158.997795151368,-158.497802084854,
-157.99780901834,-157.497815951827,-156.997822885313,-156.497829818799,
-155.997836752285,-155.497843685772,-154.997850619258,-154.888989121148),
 .UNSPECIFIED.);
#1238=B_SPLINE_CURVE_WITH_KNOTS('',3,(#29401,#29402,#29403,#29404,#29405,
#29406,#29407,#29408,#29409,#29410,#29411,#29412,#29413,#29414,#29415,#29416,
#29417,#29418,#29419,#29420,#29421,#29422,#29423,#29424,#29425,#29426,#29427,
#29428,#29429,#29430,#29431,#29432,#29433,#29434,#29435,#29436,#29437,#29438,
#29439,#29440,#29441,#29442,#29443),.UNSPECIFIED.,.F.,.F.,(4,3,3,3,3,3,
3,3,3,3,3,3,3,3,4),(151.915302465848,151.997892220175,152.497885286689,
152.997878353203,153.497871419717,153.99786448623,154.497857552744,154.997850619258,
155.497843685772,155.997836752285,156.497829818799,156.997822885313,157.497815951827,
157.99780901834,158.198487773028),.UNSPECIFIED.);
#1239=B_SPLINE_CURVE_WITH_KNOTS('',3,(#29448,#29449,#29450,#29451,#29452,
#29453,#29454,#29455,#29456,#29457,#29458,#29459,#29460,#29461,#29462,#29463,
#29464,#29465,#29466,#29467,#29468,#29469,#29470,#29471,#29472,#29473,#29474,
#29475,#29476,#29477,#29478,#29479,#29480,#29481,#29482,#29483,#29484,#29485,
#29486,#29487),.UNSPECIFIED.,.F.,.F.,(4,3,3,3,3,3,3,3,3,3,3,3,3,4),(-167.455359735507,
-166.997684215588,-166.497691149074,-165.99769808256,-165.497705016046,
-164.997711949533,-164.497718883019,-163.997725816505,-163.497732749991,
-162.997739683478,-162.497746616964,-161.99775355045,-161.497760483937,
-161.172174428328),.UNSPECIFIED.);
#1240=B_SPLINE_CURVE_WITH_KNOTS('',3,(#29488,#29489,#29490,#29491,#29492,
#29493,#29494,#29495,#29496,#29497,#29498,#29499,#29500,#29501,#29502,#29503,
#29504,#29505,#29506,#29507,#29508,#29509,#29510,#29511,#29512,#29513,#29514,
#29515,#29516,#29517,#29518,#29519,#29520,#29521,#29522,#29523,#29524,#29525,
#29526,#29527),.UNSPECIFIED.,.F.,.F.,(4,3,3,3,3,3,3,3,3,3,3,3,3,4),(158.198487773028,
158.497802084854,158.997795151368,159.497788217882,159.997781284395,160.497774350909,
160.997767417423,161.497760483937,161.99775355045,162.497746616964,162.997739683478,
163.497732749991,163.997725816505,164.481673080207),.UNSPECIFIED.);
#1241=B_SPLINE_CURVE_WITH_KNOTS('',3,(#29532,#29533,#29534,#29535,#29536,
#29537,#29538,#29539,#29540,#29541,#29542,#29543,#29544,#29545,#29546,#29547,
#29548,#29549,#29550,#29551,#29552,#29553,#29554,#29555,#29556,#29557,#29558,
#29559,#29560,#29561,#29562,#29563,#29564,#29565,#29566,#29567,#29568,#29569,
#29570,#29571,#29572,#29573,#29574),.UNSPECIFIED.,.F.,.F.,(4,3,3,3,3,3,
3,3,3,3,3,3,3,3,4),(-173.738545042687,-173.497594080266,-172.997601013752,
-172.497607947239,-171.997614880725,-171.497621814211,-170.997628747697,
-170.497635681184,-169.99764261467,-169.497649548156,-168.997656481642,
-168.497663415129,-167.997670348615,-167.497677282101,-167.455359735507),
 .UNSPECIFIED.);
#1242=B_SPLINE_CURVE_WITH_KNOTS('',3,(#29575,#29576,#29577,#29578,#29579,
#29580,#29581,#29582,#29583,#29584,#29585,#29586,#29587,#29588,#29589,#29590,
#29591,#29592,#29593,#29594,#29595,#29596,#29597,#29598,#29599,#29600,#29601,
#29602,#29603,#29604,#29605,#29606,#29607,#29608,#29609,#29610,#29611,#29612,
#29613,#29614,#29615,#29616,#29617),.UNSPECIFIED.,.F.,.F.,(4,3,3,3,3,3,
3,3,3,3,3,3,3,3,4),(164.481673080207,164.497718883019,164.997711949533,
165.497705016046,165.99769808256,166.497691149074,166.997684215588,167.497677282101,
167.997670348615,168.497663415129,168.997656481643,169.497649548156,169.99764261467,
170.497635681184,170.764858387387),.UNSPECIFIED.);
#1243=B_SPLINE_CURVE_WITH_KNOTS('',3,(#29622,#29623,#29624,#29625,#29626,
#29627,#29628,#29629,#29630,#29631,#29632,#29633,#29634,#29635,#29636,#29637,
#29638,#29639,#29640,#29641,#29642,#29643,#29644,#29645,#29646,#29647,#29648,
#29649,#29650,#29651,#29652,#29653,#29654,#29655,#29656,#29657,#29658,#29659,
#29660,#29661,#29662,#29663,#29664),.UNSPECIFIED.,.F.,.F.,(4,3,3,3,3,3,
3,3,3,3,3,3,3,3,4),(-180.021730349867,-179.997503944945,-179.497510878431,
-178.997517811917,-178.497524745403,-177.99753167889,-177.497538612376,
-176.997545545862,-176.497552479348,-175.997559412835,-175.497566346321,
-174.997573279807,-174.497580213294,-173.99758714678,-173.738545042687),
 .UNSPECIFIED.);
#1244=B_SPLINE_CURVE_WITH_KNOTS('',3,(#29665,#29666,#29667,#29668,#29669,
#29670,#29671,#29672,#29673,#29674,#29675,#29676,#29677,#29678,#29679,#29680,
#29681,#29682,#29683,#29684,#29685,#29686,#29687,#29688,#29689,#29690,#29691,
#29692,#29693,#29694,#29695,#29696,#29697,#29698,#29699,#29700,#29701,#29702,
#29703,#29704,#29705,#29706,#29707),.UNSPECIFIED.,.F.,.F.,(4,3,3,3,3,3,
3,3,3,3,3,3,3,3,4),(170.764858387387,170.997628747697,171.497621814211,
171.997614880725,172.497607947239,172.997601013752,173.497594080266,173.99758714678,
174.497580213294,174.997573279807,175.497566346321,175.997559412835,176.497552479349,
176.997545545862,177.048043694566),.UNSPECIFIED.);
#1245=B_SPLINE_CURVE_WITH_KNOTS('',3,(#29712,#29713,#29714,#29715,#29716,
#29717,#29718,#29719,#29720,#29721,#29722,#29723,#29724,#29725,#29726,#29727,
#29728,#29729,#29730,#29731,#29732,#29733,#29734,#29735,#29736,#29737,#29738,
#29739,#29740,#29741,#29742,#29743,#29744,#29745,#29746,#29747,#29748,#29749,
#29750,#29751),.UNSPECIFIED.,.F.,.F.,(4,3,3,3,3,3,3,3,3,3,3,3,3,4),(-186.304915657046,
-185.997420743109,-185.497427676596,-184.997434610082,-184.497441543568,
-183.997448477055,-183.497455410541,-182.997462344027,-182.497469277513,
-181.997476211,-181.497483144486,-180.997490077972,-180.497497011458,-180.021730349867),
 .UNSPECIFIED.);
#1246=B_SPLINE_CURVE_WITH_KNOTS('',3,(#29752,#29753,#29754,#29755,#29756,
#29757,#29758,#29759,#29760,#29761,#29762,#29763,#29764,#29765,#29766,#29767,
#29768,#29769,#29770,#29771,#29772,#29773,#29774,#29775,#29776,#29777,#29778,
#29779,#29780,#29781,#29782,#29783,#29784,#29785,#29786,#29787,#29788,#29789,
#29790,#29791),.UNSPECIFIED.,.F.,.F.,(4,3,3,3,3,3,3,3,3,3,3,3,3,4),(177.048043694566,
177.497538612376,177.99753167889,178.497524745403,178.997517811917,179.497510878431,
179.997503944945,180.497497011458,180.997490077972,181.497483144486,181.997476211,
182.497469277513,182.997462344027,183.331229001746),.UNSPECIFIED.);
#1247=B_SPLINE_CURVE_WITH_KNOTS('',3,(#29796,#29797,#29798,#29799,#29800,
#29801,#29802,#29803,#29804,#29805,#29806,#29807,#29808,#29809,#29810,#29811,
#29812,#29813,#29814,#29815,#29816,#29817,#29818,#29819,#29820,#29821,#29822,
#29823,#29824,#29825,#29826,#29827,#29828,#29829,#29830,#29831,#29832,#29833,
#29834,#29835,#29836,#29837,#29838),.UNSPECIFIED.,.F.,.F.,(4,3,3,3,3,3,
3,3,3,3,3,3,3,3,4),(-192.588100964226,-192.497330607788,-191.997337541274,
-191.497344474761,-190.997351408247,-190.497358341733,-189.997365275219,
-189.497372208706,-188.997379142192,-188.497386075678,-187.997393009164,
-187.497399942651,-186.997406876137,-186.497413809623,-186.304915657046),
 .UNSPECIFIED.);
#1248=B_SPLINE_CURVE_WITH_KNOTS('',3,(#29839,#29840,#29841,#29842,#29843,
#29844,#29845,#29846,#29847,#29848,#29849,#29850,#29851,#29852,#29853,#29854,
#29855,#29856,#29857,#29858,#29859,#29860,#29861,#29862,#29863,#29864,#29865,
#29866,#29867,#29868,#29869,#29870,#29871,#29872,#29873,#29874,#29875,#29876,
#29877,#29878,#29879,#29880,#29881),.UNSPECIFIED.,.F.,.F.,(4,3,3,3,3,3,
3,3,3,3,3,3,3,3,4),(183.331229001746,183.497455410541,183.997448477055,
184.497441543568,184.997434610082,185.497427676596,185.99742074311,186.497413809623,
186.997406876137,187.497399942651,187.997393009164,188.497386075678,188.997379142192,
189.497372208706,189.614414308925),.UNSPECIFIED.);
#1249=B_SPLINE_CURVE_WITH_KNOTS('',3,(#29886,#29887,#29888,#29889,#29890,
#29891,#29892,#29893,#29894,#29895,#29896,#29897,#29898,#29899,#29900,#29901,
#29902,#29903,#29904,#29905,#29906,#29907,#29908,#29909,#29910,#29911,#29912,
#29913,#29914,#29915,#29916,#29917,#29918,#29919,#29920,#29921,#29922,#29923,
#29924,#29925),.UNSPECIFIED.,.F.,.F.,(4,3,3,3,3,3,3,3,3,3,3,3,3,4),(-198.871286271405,
-198.497247405953,-197.997254339439,-197.497261272925,-196.997268206412,
-196.497275139898,-195.997282073384,-195.49728900687,-194.997295940357,
-194.497302873843,-193.997309807329,-193.497316740816,-192.997323674302,
-192.588100964226),.UNSPECIFIED.);
#1250=B_SPLINE_CURVE_WITH_KNOTS('',3,(#29926,#29927,#29928,#29929,#29930,
#29931,#29932,#29933,#29934,#29935,#29936,#29937,#29938,#29939,#29940,#29941,
#29942,#29943,#29944,#29945,#29946,#29947,#29948,#29949,#29950,#29951,#29952,
#29953,#29954,#29955,#29956,#29957,#29958,#29959,#29960,#29961,#29962,#29963,
#29964,#29965),.UNSPECIFIED.,.F.,.F.,(4,3,3,3,3,3,3,3,3,3,3,3,3,4),(189.614414308925,
189.997365275219,190.497358341733,190.997351408247,191.497344474761,191.997337541274,
192.497330607788,192.997323674302,193.497316740816,193.997309807329,194.497302873843,
194.997295940357,195.49728900687,195.897599616105),.UNSPECIFIED.);
#1251=B_SPLINE_CURVE_WITH_KNOTS('',3,(#29970,#29971,#29972,#29973,#29974,
#29975,#29976,#29977,#29978,#29979,#29980,#29981,#29982,#29983,#29984,#29985,
#29986,#29987,#29988,#29989,#29990,#29991,#29992,#29993,#29994,#29995,#29996,
#29997,#29998,#29999,#30000,#30001,#30002,#30003,#30004,#30005,#30006,#30007,
#30008,#30009,#30010,#30011,#30012),.UNSPECIFIED.,.F.,.F.,(4,3,3,3,3,3,
3,3,3,3,3,3,3,3,4),(-205.154471578585,-204.997157270631,-204.497164204118,
-203.997171137604,-203.49717807109,-202.997185004576,-202.497191938063,
-201.997198871549,-201.497205805035,-200.997212738522,-200.497219672008,
-199.997226605494,-199.49723353898,-198.997240472467,-198.871286271405),
 .UNSPECIFIED.);
#1252=B_SPLINE_CURVE_WITH_KNOTS('',3,(#30013,#30014,#30015,#30016,#30017,
#30018,#30019,#30020,#30021,#30022,#30023,#30024,#30025,#30026,#30027,#30028,
#30029,#30030,#30031,#30032,#30033,#30034,#30035,#30036,#30037,#30038,#30039,
#30040,#30041,#30042,#30043,#30044,#30045,#30046,#30047,#30048,#30049,#30050,
#30051,#30052,#30053,#30054,#30055),.UNSPECIFIED.,.F.,.F.,(4,3,3,3,3,3,
3,3,3,3,3,3,3,3,4),(195.897599616105,195.997282073384,196.497275139898,
196.997268206412,197.497261272925,197.997254339439,198.497247405953,198.997240472467,
199.49723353898,199.997226605494,200.497219672008,200.997212738522,201.497205805035,
201.997198871549,202.180784923285),.UNSPECIFIED.);
#1253=B_SPLINE_CURVE_WITH_KNOTS('',3,(#30060,#30061,#30062,#30063,#30064,
#30065,#30066,#30067,#30068,#30069,#30070,#30071,#30072,#30073,#30074,#30075,
#30076,#30077,#30078,#30079,#30080,#30081,#30082,#30083,#30084,#30085,#30086,
#30087,#30088,#30089,#30090,#30091,#30092,#30093,#30094,#30095,#30096,#30097,
#30098,#30099),.UNSPECIFIED.,.F.,.F.,(4,3,3,3,3,3,3,3,3,3,3,3,3,4),(-211.437656885764,
-210.997074068796,-210.497081002283,-209.997087935769,-209.497094869255,
-208.997101802741,-208.497108736228,-207.997115669714,-207.4971226032,-206.997129536686,
-206.497136470173,-205.997143403659,-205.497150337145,-205.154471578585),
 .UNSPECIFIED.);
#1254=B_SPLINE_CURVE_WITH_KNOTS('',3,(#30100,#30101,#30102,#30103,#30104,
#30105,#30106,#30107,#30108,#30109,#30110,#30111,#30112,#30113,#30114,#30115,
#30116,#30117,#30118,#30119,#30120,#30121,#30122,#30123,#30124,#30125,#30126,
#30127,#30128,#30129,#30130,#30131,#30132,#30133,#30134,#30135,#30136,#30137,
#30138,#30139),.UNSPECIFIED.,.F.,.F.,(4,3,3,3,3,3,3,3,3,3,3,3,3,4),(202.180784923285,
202.497191938063,202.997185004576,203.49717807109,203.997171137604,204.497164204118,
204.997157270631,205.497150337145,205.997143403659,206.497136470173,206.997129536686,
207.4971226032,207.997115669714,208.463970230464),.UNSPECIFIED.);
#1255=B_SPLINE_CURVE_WITH_KNOTS('',3,(#30145,#30146,#30147,#30148,#30149,
#30150,#30151,#30152,#30153),.UNSPECIFIED.,.F.,.F.,(4,1,1,1,1,1,4),(223.053078404875,
223.112488654421,223.612481720935,224.112474787448,224.612467853962,225.112460920476,
225.542622064258),.UNSPECIFIED.);
#1256=B_SPLINE_CURVE_WITH_KNOTS('',3,(#30156,#30157,#30158,#30159,#30160,
#30161),.UNSPECIFIED.,.F.,.F.,(4,1,1,4),(223.053078404875,223.302941468138,
223.802934534652,224.302927601166),.UNSPECIFIED.);
#1257=B_SPLINE_CURVE_WITH_KNOTS('',3,(#30166,#30167,#30168,#30169,#30170,
#30171,#30172,#30173,#30174,#30175,#30176,#30177,#30178,#30179,#30180,#30181),
 .UNSPECIFIED.,.F.,.F.,(4,1,1,1,1,1,1,1,1,1,1,1,1,4),(216.769893097696,
217.112571856256,217.61256492277,218.112557989284,218.612551055797,219.112544122311,
219.612537188825,220.112530255338,220.612523321852,221.112516388366,221.61250945488,
222.112502521393,222.612495587907,223.053078404875),.UNSPECIFIED.);
#1258=B_SPLINE_CURVE_WITH_KNOTS('',3,(#30182,#30183,#30184,#30185,#30186,
#30187,#30188,#30189,#30190,#30191,#30192,#30193,#30194,#30195,#30196,#30197,
#30198),.UNSPECIFIED.,.F.,.F.,(4,1,1,1,1,1,1,1,1,1,1,1,1,1,4),(216.769893097696,
216.80303160346,217.303024669973,217.803017736487,218.303010803001,218.803003869514,
219.302996936028,219.802990002542,220.302983069056,220.802976135569,221.302969202083,
221.802962268597,222.302955335111,222.802948401624,223.053078404875),
 .UNSPECIFIED.);
#1259=B_SPLINE_CURVE_WITH_KNOTS('',3,(#30203,#30204,#30205,#30206,#30207,
#30208,#30209,#30210,#30211,#30212,#30213,#30214,#30215,#30216,#30217,#30218,
#30219),.UNSPECIFIED.,.F.,.F.,(4,1,1,1,1,1,1,1,1,1,1,1,1,1,4),(210.486707790516,
210.612661991577,211.112655058091,211.612648124605,212.112641191119,212.612634257632,
213.112627324146,213.61262039066,214.112613457174,214.612606523687,215.112599590201,
215.612592656715,216.112585723229,216.612578789742,216.769893097696),
 .UNSPECIFIED.);
#1260=B_SPLINE_CURVE_WITH_KNOTS('',3,(#30220,#30221,#30222,#30223,#30224,
#30225,#30226,#30227,#30228,#30229,#30230,#30231,#30232,#30233,#30234,#30235),
 .UNSPECIFIED.,.F.,.F.,(4,1,1,1,1,1,1,1,1,1,1,1,1,4),(210.486707790516,
210.803114805295,211.303107871808,211.803100938322,212.303094004836,212.80308707135,
213.303080137863,213.803073204377,214.303066270891,214.803059337405,215.303052403918,
215.803045470432,216.303038536946,216.769893097696),.UNSPECIFIED.);
#1261=B_SPLINE_CURVE_WITH_KNOTS('',3,(#30240,#30241,#30242,#30243,#30244,
#30245,#30246,#30247,#30248,#30249,#30250,#30251,#30252,#30253,#30254,#30255),
 .UNSPECIFIED.,.F.,.F.,(4,1,1,1,1,1,1,1,1,1,1,1,1,4),(204.203522483337,
204.612745193413,205.112738259926,205.61273132644,206.112724392954,206.612717459468,
207.112710525981,207.612703592495,208.112696659009,208.612689725523,209.112682792036,
209.61267585855,210.112668925064,210.486707790516),.UNSPECIFIED.);
#1262=B_SPLINE_CURVE_WITH_KNOTS('',3,(#30256,#30257,#30258,#30259,#30260,
#30261,#30262,#30263,#30264,#30265,#30266,#30267,#30268,#30269,#30270,#30271,
#30272),.UNSPECIFIED.,.F.,.F.,(4,1,1,1,1,1,1,1,1,1,1,1,1,1,4),(204.203522483337,
204.303204940616,204.80319800713,205.303191073644,205.803184140157,206.303177206671,
206.803170273185,207.303163339699,207.803156406212,208.303149472726,208.80314253924,
209.303135605754,209.803128672267,210.303121738781,210.486707790516),
 .UNSPECIFIED.);
#1263=B_SPLINE_CURVE_WITH_KNOTS('',3,(#30277,#30278,#30279,#30280,#30281,
#30282,#30283,#30284,#30285,#30286,#30287,#30288,#30289,#30290,#30291,#30292,
#30293),.UNSPECIFIED.,.F.,.F.,(4,1,1,1,1,1,1,1,1,1,1,1,1,1,4),(197.920337176157,
198.112835328734,198.612828395248,199.112821461762,199.612814528275,200.112807594789,
200.612800661303,201.112793727816,201.61278679433,202.112779860844,202.612772927358,
203.112765993871,203.612759060385,204.112752126899,204.203522483337),
 .UNSPECIFIED.);
#1264=B_SPLINE_CURVE_WITH_KNOTS('',3,(#30294,#30295,#30296,#30297,#30298,
#30299,#30300,#30301,#30302,#30303,#30304,#30305,#30306,#30307,#30308,#30309),
 .UNSPECIFIED.,.F.,.F.,(4,1,1,1,1,1,1,1,1,1,1,1,1,4),(197.920337176157,
198.303288142451,198.803281208965,199.303274275479,199.803267341993,200.303260408506,
200.80325347502,201.303246541534,201.803239608047,202.303232674561,202.803225741075,
203.303218807589,203.803211874102,204.203522483337),.UNSPECIFIED.);
#1265=B_SPLINE_CURVE_WITH_KNOTS('',3,(#30314,#30315,#30316,#30317,#30318,
#30319,#30320,#30321,#30322,#30323,#30324,#30325,#30326,#30327,#30328,#30329),
 .UNSPECIFIED.,.F.,.F.,(4,1,1,1,1,1,1,1,1,1,1,1,1,4),(191.637151868977,
192.112918530569,192.612911597083,193.112904663597,193.61289773011,194.112890796624,
194.612883863138,195.112876929652,195.612869996165,196.112863062679,196.612856129193,
197.112849195707,197.61284226222,197.920337176157),.UNSPECIFIED.);
#1266=B_SPLINE_CURVE_WITH_KNOTS('',3,(#30330,#30331,#30332,#30333,#30334,
#30335,#30336,#30337,#30338,#30339,#30340,#30341,#30342,#30343,#30344,#30345,
#30346),.UNSPECIFIED.,.F.,.F.,(4,1,1,1,1,1,1,1,1,1,1,1,1,1,4),(191.637151868977,
191.803378277773,192.303371344287,192.8033644108,193.303357477314,193.803350543828,
194.303343610341,194.803336676855,195.303329743369,195.803322809883,196.303315876396,
196.80330894291,197.303302009424,197.803295075938,197.920337176157),
 .UNSPECIFIED.);
#1267=B_SPLINE_CURVE_WITH_KNOTS('',3,(#30351,#30352,#30353,#30354,#30355,
#30356,#30357,#30358,#30359,#30360,#30361,#30362,#30363,#30364,#30365,#30366,
#30367),.UNSPECIFIED.,.F.,.F.,(4,1,1,1,1,1,1,1,1,1,1,1,1,1,4),(185.353966561798,
185.613008665891,186.113001732404,186.612994798918,187.112987865432,187.612980931946,
188.112973998459,188.612967064973,189.112960131487,189.612953198001,190.112946264514,
190.612939331028,191.112932397542,191.612925464056,191.637151868977),
 .UNSPECIFIED.);
#1268=B_SPLINE_CURVE_WITH_KNOTS('',3,(#30368,#30369,#30370,#30371,#30372,
#30373,#30374,#30375,#30376,#30377,#30378,#30379,#30380,#30381,#30382,#30383),
 .UNSPECIFIED.,.F.,.F.,(4,1,1,1,1,1,1,1,1,1,1,1,1,4),(185.353966561798,
185.803461479608,186.303454546122,186.803447612635,187.303440679149,187.803433745663,
188.303426812177,188.80341987869,189.303412945204,189.803406011718,190.303399078232,
190.803392144745,191.303385211259,191.637151868977),.UNSPECIFIED.);
#1269=B_SPLINE_CURVE_WITH_KNOTS('',3,(#30388,#30389,#30390,#30391,#30392,
#30393,#30394,#30395,#30396,#30397,#30398,#30399,#30400,#30401,#30402,#30403,
#30404),.UNSPECIFIED.,.F.,.F.,(4,1,1,1,1,1,1,1,1,1,1,1,1,1,4),(179.070781254618,
179.113098801212,179.613091867726,180.11308493424,180.613078000753,181.113071067267,
181.613064133781,182.113057200295,182.613050266808,183.113043333322,183.613036399836,
184.11302946635,184.613022532863,185.113015599377,185.353966561798),
 .UNSPECIFIED.);
#1270=B_SPLINE_CURVE_WITH_KNOTS('',3,(#30405,#30406,#30407,#30408,#30409,
#30410,#30411,#30412,#30413,#30414,#30415,#30416,#30417,#30418,#30419,#30420,
#30421),.UNSPECIFIED.,.F.,.F.,(4,1,1,1,1,1,1,1,1,1,1,1,1,1,4),(179.070781254618,
179.303551614929,179.803544681443,180.303537747957,180.803530814471,181.303523880984,
181.803516947498,182.303510014012,182.803503080526,183.303496147039,183.803489213553,
184.303482280067,184.803475346581,185.303468413094,185.353966561798),
 .UNSPECIFIED.);
#1271=B_SPLINE_CURVE_WITH_KNOTS('',3,(#30426,#30427,#30428,#30429,#30430,
#30431,#30432,#30433,#30434,#30435,#30436,#30437,#30438,#30439,#30440,#30441),
 .UNSPECIFIED.,.F.,.F.,(4,1,1,1,1,1,1,1,1,1,1,1,1,4),(172.787595947439,
173.113182003047,173.613175069561,174.113168136075,174.613161202589,175.113154269102,
175.613147335616,176.11314040213,176.613133468643,177.113126535157,177.613119601671,
178.113112668185,178.613105734698,179.070781254618),.UNSPECIFIED.);
#1272=B_SPLINE_CURVE_WITH_KNOTS('',3,(#30442,#30443,#30444,#30445,#30446,
#30447,#30448,#30449,#30450,#30451,#30452,#30453,#30454,#30455,#30456,#30457,
#30458),.UNSPECIFIED.,.F.,.F.,(4,1,1,1,1,1,1,1,1,1,1,1,1,1,4),(172.787595947439,
172.803641750251,173.303634816765,173.803627883278,174.303620949792,174.803614016306,
175.30360708282,175.803600149333,176.303593215847,176.803586282361,177.303579348874,
177.803572415388,178.303565481902,178.803558548416,179.070781254618),
 .UNSPECIFIED.);
#1273=B_SPLINE_CURVE_WITH_KNOTS('',3,(#30463,#30464,#30465,#30466,#30467,
#30468,#30469,#30470,#30471,#30472,#30473,#30474,#30475,#30476,#30477,#30478,
#30479),.UNSPECIFIED.,.F.,.F.,(4,1,1,1,1,1,1,1,1,1,1,1,1,1,4),(166.504410640259,
166.613272138369,167.113265204883,167.613258271396,168.11325133791,168.613244404424,
169.113237470937,169.613230537451,170.113223603965,170.613216670479,171.113209736992,
171.613202803506,172.11319587002,172.613188936534,172.787595947439),
 .UNSPECIFIED.);
#1274=B_SPLINE_CURVE_WITH_KNOTS('',3,(#30480,#30481,#30482,#30483,#30484,
#30485,#30486,#30487,#30488,#30489,#30490,#30491,#30492,#30493,#30494,#30495),
 .UNSPECIFIED.,.F.,.F.,(4,1,1,1,1,1,1,1,1,1,1,1,1,4),(166.504410640259,
166.803724952086,167.3037180186,167.803711085113,168.303704151627,168.803697218141,
169.303690284655,169.803683351168,170.303676417682,170.803669484196,171.30366255071,
171.803655617223,172.303648683737,172.787595947439),.UNSPECIFIED.);
#1275=B_SPLINE_CURVE_WITH_KNOTS('',3,(#30500,#30501,#30502,#30503,#30504,
#30505,#30506,#30507,#30508,#30509,#30510,#30511,#30512,#30513,#30514,#30515),
 .UNSPECIFIED.,.F.,.F.,(4,1,1,1,1,1,1,1,1,1,1,1,1,4),(160.22122533308,160.613355340204,
161.113348406718,161.613341473231,162.113334539745,162.613327606259,163.113320672773,
163.613313739286,164.1133068058,164.613299872314,165.113292938828,165.613286005341,
166.113279071855,166.504410640259),.UNSPECIFIED.);
#1276=B_SPLINE_CURVE_WITH_KNOTS('',3,(#30516,#30517,#30518,#30519,#30520,
#30521,#30522,#30523,#30524,#30525,#30526,#30527,#30528,#30529,#30530,#30531,
#30532),.UNSPECIFIED.,.F.,.F.,(4,1,1,1,1,1,1,1,1,1,1,1,1,1,4),(160.22122533308,
160.303815087407,160.803808153921,161.303801220435,161.803794286949,162.303787353462,
162.803780419976,163.30377348649,163.803766553004,164.303759619517,164.803752686031,
165.303745752545,165.803738819059,166.303731885572,166.504410640259),
 .UNSPECIFIED.);
#1277=B_SPLINE_CURVE_WITH_KNOTS('',3,(#30537,#30538,#30539,#30540,#30541,
#30542,#30543,#30544,#30545,#30546,#30547,#30548,#30549,#30550,#30551,#30552,
#30553),.UNSPECIFIED.,.F.,.F.,(4,1,1,1,1,1,1,1,1,1,1,1,1,1,4),(153.9380400259,
154.113445475525,154.613438542039,155.113431608553,155.613424675067,156.11341774158,
156.613410808094,157.113403874608,157.613396941122,158.113390007635,158.613383074149,
159.113376140663,159.613369207177,160.11336227369,160.22122533308),
 .UNSPECIFIED.);
#1278=B_SPLINE_CURVE_WITH_KNOTS('',3,(#30554,#30555,#30556,#30557,#30558,
#30559,#30560,#30561,#30562,#30563,#30564,#30565,#30566,#30567,#30568,#30569),
 .UNSPECIFIED.,.F.,.F.,(4,1,1,1,1,1,1,1,1,1,1,1,1,4),(153.9380400259,154.303898289243,
154.803891355756,155.30388442227,155.803877488784,156.303870555298,156.803863621811,
157.303856688325,157.803849754839,158.303842821353,158.803835887866,159.30382895438,
159.803822020894,160.22122533308),.UNSPECIFIED.);
#1279=B_SPLINE_CURVE_WITH_KNOTS('',3,(#30574,#30575,#30576,#30577,#30578,
#30579,#30580,#30581,#30582,#30583,#30584,#30585,#30586,#30587,#30588,#30589),
 .UNSPECIFIED.,.F.,.F.,(4,1,1,1,1,1,1,1,1,1,1,1,1,4),(147.65485471872,148.113528677361,
148.613521743874,149.113514810388,149.613507876902,150.113500943416,150.613494009929,
151.113487076443,151.613480142957,152.11347320947,152.613466275984,153.113459342498,
153.613452409012,153.9380400259),.UNSPECIFIED.);
#1280=B_SPLINE_CURVE_WITH_KNOTS('',3,(#30590,#30591,#30592,#30593,#30594,
#30595,#30596,#30597,#30598,#30599,#30600,#30601,#30602,#30603,#30604,#30605,
#30606),.UNSPECIFIED.,.F.,.F.,(4,1,1,1,1,1,1,1,1,1,1,1,1,1,4),(147.654854718721,
147.803988424564,148.303981491078,148.803974557592,149.303967624105,149.803960690619,
150.303953757133,150.803946823646,151.30393989016,151.803932956674,152.303926023188,
152.803919089701,153.303912156215,153.803905222729,153.9380400259),
 .UNSPECIFIED.);
#1281=B_SPLINE_CURVE_WITH_KNOTS('',3,(#30611,#30612,#30613,#30614,#30615,
#30616,#30617,#30618,#30619,#30620,#30621,#30622,#30623,#30624,#30625,#30626,
#30627),.UNSPECIFIED.,.F.,.F.,(4,1,1,1,1,1,1,1,1,1,1,1,1,1,4),(141.371669411541,
141.613618812682,142.113611879196,142.61360494571,143.113598012223,143.613591078737,
144.113584145251,144.613577211764,145.113570278278,145.613563344792,146.113556411306,
146.613549477819,147.113542544333,147.613535610847,147.65485471872),
 .UNSPECIFIED.);
#1282=B_SPLINE_CURVE_WITH_KNOTS('',3,(#30628,#30629,#30630,#30631,#30632,
#30633,#30634,#30635,#30636,#30637,#30638,#30639,#30640,#30641,#30642,#30643),
 .UNSPECIFIED.,.F.,.F.,(4,1,1,1,1,1,1,1,1,1,1,1,1,4),(141.371669411541,
141.804071626399,142.304064692913,142.804057759427,143.30405082594,143.804043892454,
144.304036958968,144.804030025482,145.304023091995,145.804016158509,146.304009225023,
146.804002291537,147.30399535805,147.654854718721),.UNSPECIFIED.);
#1283=B_SPLINE_CURVE_WITH_KNOTS('',3,(#30648,#30649,#30650,#30651,#30652,
#30653,#30654,#30655,#30656,#30657,#30658,#30659,#30660,#30661,#30662,#30663,
#30664),.UNSPECIFIED.,.F.,.F.,(4,1,1,1,1,1,1,1,1,1,1,1,1,1,4),(135.088484104361,
135.113708948003,135.613702014517,136.113695081031,136.613688147545,137.113681214058,
137.613674280572,138.113667347086,138.6136604136,139.113653480113,139.613646546627,
140.113639613141,140.613632679655,141.113625746168,141.371669411541),
 .UNSPECIFIED.);
#1284=B_SPLINE_CURVE_WITH_KNOTS('',3,(#30665,#30666,#30667,#30668,#30669,
#30670,#30671,#30672,#30673,#30674,#30675,#30676,#30677,#30678,#30679,#30680,
#30681),.UNSPECIFIED.,.F.,.F.,(4,1,1,1,1,1,1,1,1,1,1,1,1,1,4),(135.088484104361,
135.304161761721,135.804154828234,136.304147894748,136.804140961262,137.304134027776,
137.804127094289,138.304120160803,138.804113227317,139.304106293831,139.804099360344,
140.304092426858,140.804085493372,141.304078559886,141.371669411541),
 .UNSPECIFIED.);
#1285=B_SPLINE_CURVE_WITH_KNOTS('',3,(#30686,#30687,#30688,#30689,#30690,
#30691,#30692,#30693,#30694,#30695,#30696,#30697,#30698,#30699,#30700,#30701),
 .UNSPECIFIED.,.F.,.F.,(4,1,1,1,1,1,1,1,1,1,1,1,1,4),(128.805298797182,
129.113792149839,129.613785216352,130.113778282866,130.61377134938,131.113764415894,
131.613757482407,132.113750548921,132.613743615435,133.113736681949,133.613729748462,
134.113722814976,134.61371588149,135.088484104361),.UNSPECIFIED.);
#1286=B_SPLINE_CURVE_WITH_KNOTS('',3,(#30702,#30703,#30704,#30705,#30706,
#30707,#30708,#30709,#30710,#30711,#30712,#30713,#30714,#30715,#30716,#30717),
 .UNSPECIFIED.,.F.,.F.,(4,1,1,1,1,1,1,1,1,1,1,1,1,4),(128.805298797182,
129.304244963556,129.80423803007,130.304231096583,130.804224163097,131.304217229611,
131.804210296125,132.304203362638,132.804196429152,133.304189495666,133.80418256218,
134.304175628693,134.804168695207,135.088484104361),.UNSPECIFIED.);
#1287=B_SPLINE_CURVE_WITH_KNOTS('',3,(#30722,#30723,#30724,#30725,#30726,
#30727,#30728,#30729,#30730,#30731,#30732,#30733,#30734,#30735,#30736,#30737,
#30738),.UNSPECIFIED.,.F.,.F.,(4,1,1,1,1,1,1,1,1,1,1,1,1,1,4),(122.522113490002,
122.61388228516,123.113875351674,123.613868418188,124.113861484701,124.613854551215,
125.113847617729,125.613840684243,126.113833750756,126.61382681727,127.113819883784,
127.613812950297,128.113806016811,128.613799083325,128.805298797182),
 .UNSPECIFIED.);
#1288=B_SPLINE_CURVE_WITH_KNOTS('',3,(#30739,#30740,#30741,#30742,#30743,
#30744,#30745,#30746,#30747,#30748,#30749,#30750,#30751,#30752,#30753,#30754,
#30755),.UNSPECIFIED.,.F.,.F.,(4,1,1,1,1,1,1,1,1,1,1,1,1,1,4),(122.522113490002,
122.804335098877,123.304328165391,123.804321231905,124.304314298419,124.804307364932,
125.304300431446,125.80429349796,126.304286564473,126.804279630987,127.304272697501,
127.804265764015,128.304258830528,128.804251897042,128.805298797182),
 .UNSPECIFIED.);
#1289=B_SPLINE_CURVE_WITH_KNOTS('',3,(#30760,#30761,#30762,#30763,#30764,
#30765,#30766,#30767,#30768,#30769,#30770,#30771,#30772,#30773,#30774,#30775),
 .UNSPECIFIED.,.F.,.F.,(4,1,1,1,1,1,1,1,1,1,1,1,1,4),(116.238928182823,
116.613965486995,117.113958553509,117.613951620023,118.113944686536,118.61393775305,
119.113930819564,119.613923886078,120.113916952591,120.613910019105,121.113903085619,
121.613896152133,122.113889218646,122.522113490002),.UNSPECIFIED.);
#1290=B_SPLINE_CURVE_WITH_KNOTS('',3,(#30776,#30777,#30778,#30779,#30780,
#30781,#30782,#30783,#30784,#30785,#30786,#30787,#30788,#30789,#30790,#30791,
#30792),.UNSPECIFIED.,.F.,.F.,(4,1,1,1,1,1,1,1,1,1,1,1,1,1,4),(116.238928182823,
116.304425234199,116.804418300713,117.304411367226,117.80440443374,118.304397500254,
118.804390566767,119.304383633281,119.804376699795,120.304369766309,120.804362832822,
121.304355899336,121.80434896585,122.304342032364,122.522113490002),
 .UNSPECIFIED.);
#1291=B_SPLINE_CURVE_WITH_KNOTS('',3,(#30797,#30798,#30799,#30800,#30801,
#30802,#30803,#30804,#30805,#30806,#30807,#30808,#30809,#30810,#30811,#30812,
#30813),.UNSPECIFIED.,.F.,.F.,(4,1,1,1,1,1,1,1,1,1,1,1,1,1,4),(109.955742875643,
110.114055622317,110.61404868883,111.114041755344,111.614034821858,112.114027888372,
112.614020954885,113.114014021399,113.614007087913,114.114000154427,114.61399322094,
115.113986287454,115.613979353968,116.113972420482,116.238928182823),
 .UNSPECIFIED.);
#1292=B_SPLINE_CURVE_WITH_KNOTS('',3,(#30814,#30815,#30816,#30817,#30818,
#30819,#30820,#30821,#30822,#30823,#30824,#30825,#30826,#30827,#30828,#30829),
 .UNSPECIFIED.,.F.,.F.,(4,1,1,1,1,1,1,1,1,1,1,1,1,4),(109.955742875643,
110.304508436034,110.804501502548,111.304494569061,111.804487635575,112.304480702089,
112.804473768603,113.304466835116,113.80445990163,114.304452968144,114.804446034658,
115.304439101171,115.804432167685,116.238928182823),.UNSPECIFIED.);
#1293=B_SPLINE_CURVE_WITH_KNOTS('',3,(#30834,#30835,#30836,#30837,#30838,
#30839,#30840,#30841,#30842,#30843,#30844,#30845,#30846,#30847,#30848,#30849),
 .UNSPECIFIED.,.F.,.F.,(4,1,1,1,1,1,1,1,1,1,1,1,1,4),(103.672557568463,
104.114138824152,104.614131890666,105.114124957179,105.614118023693,106.114111090207,
106.614104156721,107.114097223234,107.614090289748,108.114083356262,108.614076422776,
109.114069489289,109.614062555803,109.955742875643),.UNSPECIFIED.);
#1294=B_SPLINE_CURVE_WITH_KNOTS('',3,(#30850,#30851,#30852,#30853,#30854,
#30855,#30856,#30857,#30858,#30859,#30860,#30861,#30862,#30863,#30864,#30865,
#30866),.UNSPECIFIED.,.F.,.F.,(4,1,1,1,1,1,1,1,1,1,1,1,1,1,4),(103.672557568463,
103.804598571355,104.304591637869,104.804584704383,105.304577770897,105.80457083741,
106.304563903924,106.804556970438,107.304550036952,107.804543103465,108.304536169979,
108.804529236493,109.304522303006,109.80451536952,109.955742875643),
 .UNSPECIFIED.);
#1295=B_SPLINE_CURVE_WITH_KNOTS('',3,(#30871,#30872,#30873,#30874,#30875,
#30876,#30877,#30878,#30879,#30880,#30881,#30882,#30883,#30884,#30885,#30886,
#30887),.UNSPECIFIED.,.F.,.F.,(4,1,1,1,1,1,1,1,1,1,1,1,1,1,4),(97.3893722612838,
97.6142289594734,98.1142220259871,98.6142150925008,99.1142081590146,99.6142012255283,
100.114194292042,100.614187358556,101.11418042507,101.614173491583,102.114166558097,
102.614159624611,103.114152691124,103.614145757638,103.672557568463),
 .UNSPECIFIED.);
#1296=B_SPLINE_CURVE_WITH_KNOTS('',3,(#30888,#30889,#30890,#30891,#30892,
#30893,#30894,#30895,#30896,#30897,#30898,#30899,#30900,#30901,#30902,#30903),
 .UNSPECIFIED.,.F.,.F.,(4,1,1,1,1,1,1,1,1,1,1,1,1,4),(97.3893722612839,
97.8046817731906,98.3046748397043,98.804667906218,99.3046609727318,99.8046540392455,
100.304647105759,100.804640172273,101.304633238787,101.8046263053,102.304619371814,
102.804612438328,103.304605504842,103.672557568463),.UNSPECIFIED.);
#1297=B_SPLINE_CURVE_WITH_KNOTS('',3,(#30908,#30909,#30910,#30911,#30912,
#30913,#30914,#30915,#30916,#30917,#30918,#30919,#30920,#30921,#30922,#30923,
#30924),.UNSPECIFIED.,.F.,.F.,(4,1,1,1,1,1,1,1,1,1,1,1,1,1,4),(91.1061869541042,
91.1143190947948,91.6143121613085,92.1143052278223,92.614298294336,93.1142913608497,
93.6142844273635,94.1142774938772,94.6142705603909,95.1142636269047,95.6142566934184,
96.1142497599322,96.6142428264459,97.1142358929596,97.3893722612838),
 .UNSPECIFIED.);
#1298=B_SPLINE_CURVE_WITH_KNOTS('',3,(#30925,#30926,#30927,#30928,#30929,
#30930,#30931,#30932,#30933,#30934,#30935,#30936,#30937,#30938,#30939,#30940,
#30941),.UNSPECIFIED.,.F.,.F.,(4,1,1,1,1,1,1,1,1,1,1,1,1,1,4),(91.1061869541043,
91.304771908512,91.8047649750257,92.3047580415395,92.8047511080532,93.3047441745669,
93.8047372410807,94.3047303075944,94.8047233741082,95.3047164406219,95.8047095071356,
96.3047025736494,96.8046956401631,97.3046887066768,97.3893722612839),
 .UNSPECIFIED.);
#1299=B_SPLINE_CURVE_WITH_KNOTS('',3,(#30946,#30947,#30948,#30949,#30950,
#30951,#30952,#30953,#30954,#30955,#30956,#30957,#30958,#30959,#30960,#30961),
 .UNSPECIFIED.,.F.,.F.,(4,1,1,1,1,1,1,1,1,1,1,1,1,4),(84.8230016469246,
85.11440229663,85.6143953631437,86.1143884296575,86.6143814961712,87.1143745626849,
87.6143676291987,88.1143606957124,88.6143537622261,89.1143468287399,89.6143398952536,
90.1143329617673,90.6143260282811,91.1061869541042),.UNSPECIFIED.);
#1300=B_SPLINE_CURVE_WITH_KNOTS('',3,(#30962,#30963,#30964,#30965,#30966,
#30967,#30968,#30969,#30970,#30971,#30972,#30973,#30974,#30975,#30976,#30977),
 .UNSPECIFIED.,.F.,.F.,(4,1,1,1,1,1,1,1,1,1,1,1,1,4),(84.8230016469247,
85.3048551103472,85.8048481768609,86.3048412433747,86.8048343098884,87.3048273764021,
87.8048204429159,88.3048135094296,88.8048065759433,89.3047996424571,89.8047927089708,
90.3047857754845,90.8047788419983,91.1061869541043),.UNSPECIFIED.);
#1301=B_SPLINE_CURVE_WITH_KNOTS('',3,(#30982,#30983,#30984,#30985,#30986,
#30987,#30988,#30989,#30990,#30991,#30992,#30993,#30994,#30995,#30996,#30997,
#30998),.UNSPECIFIED.,.F.,.F.,(4,1,1,1,1,1,1,1,1,1,1,1,1,1,4),(78.539816339745,
78.6144924319514,79.1144854984652,79.6144785649789,80.1144716314926,80.6144646980064,
81.1144577645201,81.6144508310338,82.1144438975476,82.6144369640613,83.114430030575,
83.6144230970888,84.1144161636025,84.6144092301162,84.8230016469246),
 .UNSPECIFIED.);
#1302=B_SPLINE_CURVE_WITH_KNOTS('',3,(#30999,#31000,#31001,#31002,#31003,
#31004,#31005,#31006,#31007,#31008,#31009,#31010,#31011,#31012,#31013,#31014,
#31015),.UNSPECIFIED.,.F.,.F.,(4,1,1,1,1,1,1,1,1,1,1,1,1,1,4),(78.5398163397451,
78.8049452456686,79.3049383121824,79.8049313786961,80.3049244452098,80.8049175117236,
81.3049105782373,81.804903644751,82.3048967112648,82.8048897777785,83.3048828442923,
83.804875910806,84.3048689773197,84.8048620438335,84.8230016469247),
 .UNSPECIFIED.);
#1303=B_SPLINE_CURVE_WITH_KNOTS('',3,(#31020,#31021,#31022,#31023,#31024,
#31025,#31026,#31027,#31028,#31029,#31030,#31031,#31032,#31033,#31034,#31035),
 .UNSPECIFIED.,.F.,.F.,(4,1,1,1,1,1,1,1,1,1,1,1,1,4),(72.2566310325655,
72.6145756337866,73.1145687003003,73.6145617668141,74.1145548333278,74.6145478998415,
75.1145409663553,75.614534032869,76.1145270993827,76.6145201658965,77.1145132324102,
77.614506298924,78.1144993654377,78.539816339745),.UNSPECIFIED.);
#1304=B_SPLINE_CURVE_WITH_KNOTS('',3,(#31036,#31037,#31038,#31039,#31040,
#31041,#31042,#31043,#31044,#31045,#31046,#31047,#31048,#31049,#31050,#31051,
#31052),.UNSPECIFIED.,.F.,.F.,(4,1,1,1,1,1,1,1,1,1,1,1,1,1,4),(72.2566310325655,
72.3050353809901,72.8050284475038,73.3050215140175,73.8050145805313,74.305007647045,
74.8050007135587,75.3049937800725,75.8049868465862,76.3049799131,76.8049729796137,
77.3049660461274,77.8049591126412,78.3049521791549,78.5398163397451),
 .UNSPECIFIED.);
#1305=B_SPLINE_CURVE_WITH_KNOTS('',3,(#31057,#31058,#31059,#31060,#31061,
#31062,#31063,#31064,#31065,#31066,#31067,#31068,#31069,#31070,#31071,#31072,
#31073),.UNSPECIFIED.,.F.,.F.,(4,1,1,1,1,1,1,1,1,1,1,1,1,1,4),(65.9734457253858,
66.114665769108,66.6146588356218,67.1146519021355,67.6146449686492,68.114638035163,
68.6146311016767,69.1146241681904,69.6146172347042,70.1146103012179,70.6146033677317,
71.1145964342454,71.6145895007591,72.1145825672729,72.2566310325655),
 .UNSPECIFIED.);
#1306=B_SPLINE_CURVE_WITH_KNOTS('',3,(#31074,#31075,#31076,#31077,#31078,
#31079,#31080,#31081,#31082,#31083,#31084,#31085,#31086,#31087,#31088,#31089),
 .UNSPECIFIED.,.F.,.F.,(4,1,1,1,1,1,1,1,1,1,1,1,1,4),(65.9734457253859,
66.3051185828252,66.805111649339,67.3051047158527,67.8050977823664,68.3050908488802,
68.8050839153939,69.3050769819077,69.8050700484214,70.3050631149351,70.8050561814489,
71.3050492479626,71.8050423144763,72.2566310325655),.UNSPECIFIED.);
#1307=B_SPLINE_CURVE_WITH_KNOTS('',3,(#31094,#31095,#31096,#31097,#31098,
#31099,#31100,#31101,#31102,#31103,#31104,#31105,#31106,#31107,#31108,#31109),
 .UNSPECIFIED.,.F.,.F.,(4,1,1,1,1,1,1,1,1,1,1,1,1,4),(59.6902604182063,
60.1147489709432,60.6147420374569,61.1147351039707,61.6147281704844,62.1147212369982,
62.6147143035119,63.1147073700256,63.6147004365394,64.1146935030531,64.6146865695668,
65.1146796360806,65.6146727025943,65.9734457253858),.UNSPECIFIED.);
#1308=B_SPLINE_CURVE_WITH_KNOTS('',3,(#31110,#31111,#31112,#31113,#31114,
#31115,#31116,#31117,#31118,#31119,#31120,#31121,#31122,#31123,#31124,#31125,
#31126),.UNSPECIFIED.,.F.,.F.,(4,1,1,1,1,1,1,1,1,1,1,1,1,1,4),(59.6902604182063,
59.8052087181467,60.3052017846604,60.8051948511742,61.3051879176879,61.8051809842016,
62.3051740507154,62.8051671172291,63.3051601837428,63.8051532502566,64.3051463167703,
64.805139383284,65.3051324497978,65.8051255163115,65.9734457253859),
 .UNSPECIFIED.);
#1309=B_SPLINE_CURVE_WITH_KNOTS('',3,(#31131,#31132,#31133,#31134,#31135,
#31136,#31137,#31138,#31139,#31140,#31141,#31142,#31143,#31144,#31145,#31146,
#31147),.UNSPECIFIED.,.F.,.F.,(4,1,1,1,1,1,1,1,1,1,1,1,1,1,4),(53.4070751110267,
53.6148391062647,54.1148321727784,54.6148252392921,55.1148183058059,55.6148113723196,
56.1148044388333,56.6147975053471,57.1147905718608,57.6147836383745,58.1147767048883,
58.614769771402,59.1147628379157,59.6147559044295,59.6902604182063),
 .UNSPECIFIED.);
#1310=B_SPLINE_CURVE_WITH_KNOTS('',3,(#31148,#31149,#31150,#31151,#31152,
#31153,#31154,#31155,#31156,#31157,#31158,#31159,#31160,#31161,#31162,#31163),
 .UNSPECIFIED.,.F.,.F.,(4,1,1,1,1,1,1,1,1,1,1,1,1,4),(53.4070751110267,
53.8052919199819,54.3052849864956,54.8052780530093,55.3052711195231,55.8052641860368,
56.3052572525505,56.8052503190643,57.305243385578,57.8052364520917,58.3052295186055,
58.8052225851192,59.3052156516329,59.6902604182063),.UNSPECIFIED.);
#1311=B_SPLINE_CURVE_WITH_KNOTS('',3,(#31168,#31169,#31170,#31171,#31172,
#31173,#31174,#31175,#31176,#31177,#31178,#31179,#31180,#31181,#31182,#31183),
 .UNSPECIFIED.,.F.,.F.,(4,1,1,1,1,1,1,1,1,1,1,1,1,4),(47.1238898038471,
47.6149223080998,48.1149153746136,48.6149084411273,49.114901507641,49.6148945741548,
50.1148876406685,50.6148807071823,51.114873773696,51.6148668402097,52.1148599067235,
52.6148529732372,53.1148460397509,53.4070751110267),.UNSPECIFIED.);
#1312=B_SPLINE_CURVE_WITH_KNOTS('',3,(#31184,#31185,#31186,#31187,#31188,
#31189,#31190,#31191,#31192,#31193,#31194,#31195,#31196,#31197,#31198,#31199,
#31200),.UNSPECIFIED.,.F.,.F.,(4,1,1,1,1,1,1,1,1,1,1,1,1,1,4),(47.1238898038471,
47.3053820553033,47.805375121817,48.3053681883308,48.8053612548445,49.3053543213582,
49.805347387872,50.3053404543857,50.8053335208995,51.3053265874132,51.8053196539269,
52.3053127204407,52.8053057869544,53.3052988534681,53.4070751110267),
 .UNSPECIFIED.);
#1313=B_SPLINE_CURVE_WITH_KNOTS('',3,(#31205,#31206,#31207,#31208,#31209,
#31210,#31211,#31212,#31213,#31214,#31215,#31216,#31217,#31218,#31219,#31220,
#31221),.UNSPECIFIED.,.F.,.F.,(4,1,1,1,1,1,1,1,1,1,1,1,1,1,4),(40.8407044966675,
41.1150124434213,41.615005509935,42.1149985764488,42.6149916429625,43.1149847094762,
43.61497777599,44.1149708425037,44.6149639090174,45.1149569755312,45.6149500420449,
46.1149431085586,46.6149361750724,47.1149292415861,47.1238898038471),
 .UNSPECIFIED.);
#1314=B_SPLINE_CURVE_WITH_KNOTS('',3,(#31222,#31223,#31224,#31225,#31226,
#31227,#31228,#31229,#31230,#31231,#31232,#31233,#31234,#31235,#31236,#31237),
 .UNSPECIFIED.,.F.,.F.,(4,1,1,1,1,1,1,1,1,1,1,1,1,4),(40.8407044966675,
41.3054652571385,41.8054583236522,42.305451390166,42.8054444566797,43.3054375231934,
43.8054305897072,44.3054236562209,44.8054167227346,45.3054097892484,45.8054028557621,
46.3053959222758,46.8053889887896,47.1238898038471),.UNSPECIFIED.);
#1315=B_SPLINE_CURVE_WITH_KNOTS('',3,(#31242,#31243,#31244,#31245,#31246,
#31247,#31248,#31249,#31250,#31251,#31252,#31253,#31254,#31255,#31256,#31257,
#31258),.UNSPECIFIED.,.F.,.F.,(4,1,1,1,1,1,1,1,1,1,1,1,1,1,4),(34.5575191894879,
34.6151025787427,35.1150956452565,35.6150887117702,36.1150817782839,36.6150748447977,
37.1150679113114,37.6150609778251,38.1150540443389,38.6150471108526,39.1150401773663,
39.6150332438801,40.1150263103938,40.6150193769075,40.8407044966675),
 .UNSPECIFIED.);
#1316=B_SPLINE_CURVE_WITH_KNOTS('',3,(#31259,#31260,#31261,#31262,#31263,
#31264,#31265,#31266,#31267,#31268,#31269,#31270,#31271,#31272,#31273,#31274,
#31275),.UNSPECIFIED.,.F.,.F.,(4,1,1,1,1,1,1,1,1,1,1,1,1,1,4),(34.557519189488,
34.8055553924599,35.3055484589737,35.8055415254874,36.3055345920011,36.8055276585149,
37.3055207250286,37.8055137915423,38.3055068580561,38.8054999245698,39.3054929910835,
39.8054860575973,40.305479124111,40.8054721906247,40.8407044966675),
 .UNSPECIFIED.);
#1317=B_SPLINE_CURVE_WITH_KNOTS('',3,(#31280,#31281,#31282,#31283,#31284,
#31285,#31286,#31287,#31288,#31289,#31290,#31291,#31292,#31293,#31294,#31295),
 .UNSPECIFIED.,.F.,.F.,(4,1,1,1,1,1,1,1,1,1,1,1,1,4),(28.2743338823083,
28.6151857805779,29.1151788470916,29.6151719136054,30.1151649801191,30.6151580466328,
31.1151511131466,31.6151441796603,32.115137246174,32.6151303126878,33.1151233792015,
33.6151164457153,34.115109512229,34.5575191894879),.UNSPECIFIED.);
#1318=B_SPLINE_CURVE_WITH_KNOTS('',3,(#31296,#31297,#31298,#31299,#31300,
#31301,#31302,#31303,#31304,#31305,#31306,#31307,#31308,#31309,#31310,#31311,
#31312),.UNSPECIFIED.,.F.,.F.,(4,1,1,1,1,1,1,1,1,1,1,1,1,1,4),(28.2743338823084,
28.3056455277814,28.8056385942951,29.3056316608088,29.8056247273226,30.3056177938363,
30.80561086035,31.3056039268638,31.8055969933775,32.3055900598912,32.805583126405,
33.3055761929187,33.8055692594324,34.3055623259462,34.557519189488),
 .UNSPECIFIED.);
#1319=B_SPLINE_CURVE_WITH_KNOTS('',3,(#31317,#31318,#31319,#31320,#31321,
#31322,#31323,#31324,#31325,#31326,#31327,#31328,#31329,#31330,#31331,#31332,
#31333),.UNSPECIFIED.,.F.,.F.,(4,1,1,1,1,1,1,1,1,1,1,1,1,1,4),(21.9911485751287,
22.1152759158993,22.6152689824131,23.1152620489268,23.6152551154406,24.1152481819543,
24.615241248468,25.1152343149818,25.6152273814955,26.1152204480092,26.615213514523,
27.1152065810367,27.6151996475504,28.1151927140642,28.2743338823083),
 .UNSPECIFIED.);
#1320=B_SPLINE_CURVE_WITH_KNOTS('',3,(#31334,#31335,#31336,#31337,#31338,
#31339,#31340,#31341,#31342,#31343,#31344,#31345,#31346,#31347,#31348,#31349),
 .UNSPECIFIED.,.F.,.F.,(4,1,1,1,1,1,1,1,1,1,1,1,1,4),(21.9911485751288,
22.3057287296165,22.8057217961303,23.305714862644,23.8057079291577,24.3057009956715,
24.8056940621852,25.305687128699,25.8056801952127,26.3056732617264,26.8056663282402,
27.3056593947539,27.8056524612676,28.2743338823084),.UNSPECIFIED.);
#1321=B_SPLINE_CURVE_WITH_KNOTS('',3,(#31354,#31355,#31356,#31357,#31358,
#31359,#31360,#31361,#31362,#31363,#31364,#31365,#31366,#31367,#31368,#31369),
 .UNSPECIFIED.,.F.,.F.,(4,1,1,1,1,1,1,1,1,1,1,1,1,4),(15.7079632679491,
16.1153591177345,16.6153521842483,17.115345250762,17.6153383172757,18.1153313837895,
18.6153244503032,19.1153175168169,19.6153105833307,20.1153036498444,20.6152967163581,
21.1152897828719,21.6152828493856,21.9911485751287),.UNSPECIFIED.);
#1322=B_SPLINE_CURVE_WITH_KNOTS('',3,(#31370,#31371,#31372,#31373,#31374,
#31375,#31376,#31377,#31378,#31379,#31380,#31381,#31382,#31383,#31384,#31385,
#31386),.UNSPECIFIED.,.F.,.F.,(4,1,1,1,1,1,1,1,1,1,1,1,1,1,4),(15.7079632679492,
15.805818864938,16.3058119314517,16.8058049979655,17.3057980644792,17.8057911309929,
18.3057841975067,18.8057772640204,19.3057703305341,19.8057633970479,20.3057564635616,
20.8057495300753,21.3057425965891,21.8057356631028,21.9911485751288),
 .UNSPECIFIED.);
#1323=B_SPLINE_CURVE_WITH_KNOTS('',3,(#33128,#33129,#33130,#33131,#33132,
#33133,#33134,#33135,#33136,#33137,#33138,#33139,#33140,#33141,#33142,#33143,
#33144,#33145,#33146,#33147,#33148,#33149,#33150,#33151,#33152,#33153,#33154,
#33155,#33156,#33157,#33158,#33159,#33160,#33161,#33162,#33163,#33164,#33165,
#33166,#33167,#33168,#33169,#33170,#33171,#33172,#33173,#33174,#33175,#33176,
#33177,#33178,#33179,#33180,#33181,#33182,#33183,#33184,#33185,#33186,#33187,
#33188,#33189,#33190,#33191,#33192,#33193,#33194,#33195,#33196,#33197,#33198,
#33199,#33200,#33201,#33202,#33203,#33204,#33205,#33206,#33207,#33208,#33209,
#33210,#33211,#33212,#33213,#33214,#33215,#33216,#33217,#33218,#33219,#33220,
#33221,#33222,#33223,#33224,#33225,#33226,#33227,#33228,#33229,#33230,#33231,
#33232,#33233,#33234,#33235,#33236),.UNSPECIFIED.,.F.,.F.,(4,3,3,3,3,3,
3,3,3,3,3,3,3,3,3,3,3,3,3,3,3,3,3,3,3,3,3,3,3,3,3,3,3,3,3,3,4),(-1.12653966532766,
-1.08530391285188,-1.03555276854547,-0.985995835508339,-0.97449600456723,
-0.967183168816629,-0.918323363958047,-0.869822311041264,-0.833246511105209,
-0.821905472485523,-0.815371904719748,-0.796670711169154,-0.7489242491,
-0.700999781025762,-0.653716403326253,-0.620120968748125,-0.608348915151015,
-0.601406539983964,-0.554880452923037,-0.519334665013739,-0.47261371763217,
-0.426217608843986,-0.404654224478211,-0.397976651477122,-0.39279021318813,
-0.347324068852467,-0.300517301385129,-0.25371053391779,-0.221996717178066,
-0.205387453912266,-0.194998280364054,-0.18903995937007,-0.144864377715273,
-0.100707092544083,-0.0569734759838599,-0.0141899988762762,0.),
 .UNSPECIFIED.);
#1324=B_SPLINE_CURVE_WITH_KNOTS('',3,(#33237,#33238,#33239,#33240,#33241,
#33242,#33243,#33244,#33245,#33246,#33247,#33248,#33249,#33250,#33251,#33252,
#33253,#33254,#33255,#33256,#33257,#33258,#33259,#33260,#33261,#33262,#33263,
#33264,#33265,#33266,#33267,#33268,#33269,#33270,#33271,#33272,#33273),
 .UNSPECIFIED.,.F.,.F.,(4,3,3,3,3,3,3,3,3,3,3,3,4),(208.463970230464,208.497108736228,
208.997101802741,209.497094869255,209.997087935769,210.497081002283,210.997074068796,
211.49706713531,211.997060201824,212.497053268338,212.997046334851,213.497039401365,
213.927200545147),.UNSPECIFIED.);
#1325=B_SPLINE_CURVE_WITH_KNOTS('',3,(#33275,#33276,#33277,#33278,#33279,
#33280,#33281,#33282,#33283,#33284,#33285,#33286,#33287,#33288,#33289,#33290,
#33291,#33292,#33293,#33294,#33295,#33296,#33297,#33298,#33299,#33300,#33301,
#33302,#33303,#33304,#33305,#33306,#33307,#33308,#33309,#33310,#33311,#33312,
#33313,#33314,#33315,#33316,#33317,#33318,#33319,#33320,#33321,#33322,#33323,
#33324,#33325,#33326,#33327,#33328,#33329,#33330,#33331,#33332,#33333,#33334,
#33335,#33336,#33337,#33338,#33339,#33340,#33341,#33342,#33343,#33344,#33345,
#33346,#33347,#33348,#33349,#33350,#33351,#33352,#33353,#33354,#33355,#33356,
#33357,#33358,#33359,#33360,#33361,#33362,#33363,#33364,#33365,#33366,#33367,
#33368,#33369,#33370,#33371,#33372,#33373,#33374,#33375,#33376,#33377,#33378,
#33379,#33380,#33381,#33382,#33383,#33384,#33385,#33386),.UNSPECIFIED.,
 .F.,.F.,(4,3,3,3,3,3,3,3,3,3,3,3,3,3,3,3,3,3,3,3,3,3,3,3,3,3,3,3,3,3,3,
3,3,3,3,3,3,4),(-1.13094109509778,-1.09616481350051,-1.05252904406664,-1.02447554603566,
-1.00950008969337,-1.00035998114085,-0.993301600393168,-0.94845224485129,
-0.90333045519232,-0.871780285525201,-0.865172051628852,-0.858235225141103,
-0.840230115858081,-0.795263315109601,-0.749591763211198,-0.703490048776212,
-0.670607568572991,-0.660837839774893,-0.654974428744378,-0.607853069321203,
-0.571960127963328,-0.525117783125689,-0.477884601070653,-0.454625076147963,
-0.446675645902694,-0.440719363147554,-0.39273374519351,-0.342271073441322,
-0.291808401689134,-0.255332351477992,-0.239279102906314,-0.22920132207221,
-0.222814956686309,-0.174288185380996,-0.124750052790975,-0.0750207445547947,
-0.0256773244109543,0.),.UNSPECIFIED.);
#1326=B_SPLINE_CURVE_WITH_KNOTS('',3,(#33387,#33388,#33389,#33390,#33391,
#33392,#33393,#33394,#33395,#33396,#33397,#33398,#33399,#33400),
 .UNSPECIFIED.,.F.,.F.,(4,1,1,1,1,1,1,1,1,1,1,4),(10.3757270560181,10.8058881998006,
11.3058812663144,11.8058743328281,12.3058673993418,12.8058604658556,13.3058535323693,
13.805846598883,14.3058396653968,14.8058327319105,15.3058257984242,15.7079632679492),
 .UNSPECIFIED.);
#1327=B_SPLINE_CURVE_WITH_KNOTS('',3,(#33406,#33407,#33408,#33409,#33410,
#33411,#33412,#33413,#33414,#33415,#33416,#33417,#33418,#33419,#33420,#33421,
#33422,#33423,#33424,#33425,#33426,#33427,#33428,#33429,#33430,#33431,#33432,
#33433,#33434,#33435,#33436,#33437,#33438,#33439,#33440,#33441,#33442,#33443,
#33444,#33445,#33446,#33447,#33448,#33449,#33450,#33451,#33452,#33453,#33454,
#33455,#33456,#33457,#33458,#33459,#33460,#33461,#33462,#33463,#33464,#33465,
#33466,#33467,#33468,#33469,#33470,#33471,#33472,#33473,#33474,#33475,#33476,
#33477,#33478,#33479,#33480,#33481,#33482,#33483,#33484,#33485,#33486,#33487,
#33488,#33489,#33490,#33491,#33492,#33493,#33494,#33495,#33496,#33497,#33498,
#33499,#33500,#33501,#33502,#33503,#33504,#33505,#33506,#33507,#33508,#33509,
#33510,#33511,#33512,#33513,#33514),.UNSPECIFIED.,.F.,.F.,(4,3,3,3,3,3,
3,3,3,3,3,3,3,3,3,3,3,3,3,3,3,3,3,3,3,3,3,3,3,3,3,3,3,3,3,3,4),(-1.12653966532775,
-1.08530391285196,-1.03555276855992,-0.985995835290009,-0.974496002923742,
-0.967183166935604,-0.91832336204934,-0.869822308362971,-0.833246509766086,
-0.821905469284664,-0.815371903950458,-0.7966707111692,-0.748924248651515,
-0.700999781941695,-0.653716411224205,-0.620120974671593,-0.608348933883821,
-0.601406545427275,-0.554880462036058,-0.519334665013758,-0.472613715754773,
-0.426217598085471,-0.404654215064511,-0.397976636695719,-0.39279019656135,
-0.347324049934313,-0.300517291926052,-0.253710533917792,-0.221996717178068,
-0.205387451447631,-0.194998278294185,-0.189039958905823,-0.144864372719162,
-0.100707094611733,-0.0569734906965891,-0.014190031158235,0.),
 .UNSPECIFIED.);
#1328=B_SPLINE_CURVE_WITH_KNOTS('',3,(#33517,#33518,#33519,#33520,#33521,
#33522,#33523,#33524,#33525,#33526,#33527,#33528),.UNSPECIFIED.,.F.,.F.,
(4,1,1,1,1,1,1,1,1,4),(11.6154215191109,12.1154145856246,12.6154076521384,
13.1154007186521,13.6153937851658,14.1153868516796,14.6153799181933,15.1153729847071,
15.6153660512208,15.7079632679491),.UNSPECIFIED.);
#1329=B_SPLINE_CURVE_WITH_KNOTS('',3,(#35270,#35271,#35272,#35273,#35274,
#35275,#35276,#35277,#35278,#35279,#35280,#35281,#35282,#35283,#35284,#35285,
#35286,#35287,#35288,#35289,#35290,#35291,#35292,#35293,#35294,#35295,#35296,
#35297,#35298,#35299,#35300,#35301,#35302,#35303,#35304,#35305,#35306,#35307,
#35308,#35309,#35310,#35311,#35312,#35313,#35314,#35315,#35316,#35317,#35318,
#35319,#35320,#35321,#35322,#35323,#35324,#35325,#35326,#35327,#35328,#35329,
#35330,#35331,#35332,#35333,#35334,#35335,#35336,#35337,#35338,#35339,#35340,
#35341,#35342,#35343,#35344,#35345,#35346,#35347,#35348,#35349,#35350,#35351,
#35352,#35353,#35354,#35355,#35356,#35357,#35358,#35359,#35360,#35361,#35362,
#35363,#35364,#35365,#35366,#35367,#35368,#35369,#35370,#35371,#35372,#35373,
#35374,#35375,#35376,#35377,#35378,#35379,#35380,#35381),.UNSPECIFIED.,
 .F.,.F.,(4,3,3,3,3,3,3,3,3,3,3,3,3,3,3,3,3,3,3,3,3,3,3,3,3,3,3,3,3,3,3,
3,3,3,3,3,3,4),(-1.13094109509772,-1.09616481350043,-1.05252904104694,-1.02447554499396,
-1.00950008690807,-1.00036001955662,-0.993301660201014,-0.948452303677702,
-0.903330514169959,-0.871780315013978,-0.865172021997021,-0.858235221378188,
-0.840230115857997,-0.795263319046307,-0.749591768714079,-0.703490054519165,
-0.670607572880205,-0.66083775307683,-0.654974365605059,-0.607853006298655,
-0.571960127963325,-0.52511778596238,-0.477884605450088,-0.454625079979972,
-0.446675651987665,-0.440719364207499,-0.392733749190471,-0.342271075439817,
-0.291808401689163,-0.255332351478017,-0.239279102558647,-0.229201322023436,
-0.222814957347981,-0.174288174494182,-0.124750035428491,-0.0750207266400787,
-0.025677316928006,0.),.UNSPECIFIED.);
#1330=B_SPLINE_CURVE_WITH_KNOTS('',3,(#35382,#35383,#35384,#35385,#35386,
#35387,#35388,#35389,#35390,#35391,#35392,#35393,#35394,#35395,#35396,#35397,
#35398,#35399,#35400,#35401,#35402,#35403,#35404,#35405,#35406,#35407,#35408,
#35409,#35410,#35411,#35412),.UNSPECIFIED.,.F.,.F.,(4,3,3,3,3,3,3,3,3,3,
4),(-215.997004733934,-215.49701166742,-214.997018600906,-214.497025534392,
-213.997032467879,-213.497039401365,-212.997046334851,-212.497053268337,
-211.997060201824,-211.49706713531,-211.437656885764),.UNSPECIFIED.);
#1331=B_SPLINE_CURVE_WITH_KNOTS('',3,(#36164,#36165,#36166,#36167,#36168,
#36169,#36170,#36171,#36172,#36173,#36174,#36175,#36176,#36177,#36178,#36179),
 .UNSPECIFIED.,.F.,.F.,(4,3,3,3,3,4),(-4.09323272002467,-3.93541512774918,
-3.44348823678054,-2.95156134581189,-2.45963445484324,-2.07135887395547),
 .UNSPECIFIED.);
#1332=B_SPLINE_CURVE_WITH_KNOTS('',3,(#36182,#36183,#36184,#36185,#36186,
#36187,#36188,#36189,#36190,#36191),.UNSPECIFIED.,.F.,.F.,(4,3,3,4),(0.,
0.491926890968645,0.983853781937294,1.11971880752057),.UNSPECIFIED.);
#1333=B_SPLINE_CURVE_WITH_KNOTS('',3,(#36196,#36197,#36198,#36199,#36200,
#36201,#36202,#36203,#36204,#36205,#36206,#36207,#36208,#36209,#36210,#36211,
#36212,#36213,#36214,#36215,#36216,#36217,#36218,#36219,#36220,#36221,#36222,
#36223,#36224,#36225,#36226,#36227,#36228,#36229,#36230,#36231,#36232,#36233,
#36234,#36235,#36236,#36237,#36238),.UNSPECIFIED.,.F.,.F.,(4,3,3,3,3,3,
3,3,3,3,3,3,3,3,4),(-10.3764180272043,-10.3304647103416,-9.83853781937297,
-9.34661092840432,-8.85468403743567,-8.36275714646702,-7.87083025549837,
-7.37890336452973,-6.88697647356108,-6.39504958259243,-5.90312269162378,
-5.41119580065513,-4.91926890968648,-4.42734201871783,-4.09323272002467),
 .UNSPECIFIED.);
#1334=B_SPLINE_CURVE_WITH_KNOTS('',3,(#36239,#36240,#36241,#36242,#36243,
#36244,#36245,#36246,#36247,#36248,#36249,#36250,#36251,#36252,#36253,#36254,
#36255,#36256,#36257,#36258,#36259,#36260,#36261,#36262,#36263,#36264,#36265,
#36266,#36267,#36268,#36269,#36270,#36271,#36272,#36273,#36274,#36275,#36276,
#36277,#36278,#36279,#36280,#36281),.UNSPECIFIED.,.F.,.F.,(4,3,3,3,3,3,
3,3,3,3,3,3,3,3,4),(1.11971880752057,1.47578067290594,1.96770756387459,
2.45963445484324,2.95156134581189,3.44348823678054,3.93541512774919,4.42734201871784,
4.91926890968648,5.41119580065513,5.90312269162378,6.39504958259243,6.88697647356108,
7.37890336452973,7.40290411470015),.UNSPECIFIED.);
#1335=B_SPLINE_CURVE_WITH_KNOTS('',3,(#36286,#36287,#36288,#36289,#36290,
#36291,#36292,#36293,#36294,#36295,#36296,#36297,#36298,#36299,#36300,#36301,
#36302,#36303,#36304,#36305,#36306,#36307,#36308,#36309,#36310,#36311,#36312,
#36313,#36314,#36315,#36316,#36317,#36318,#36319,#36320,#36321,#36322,#36323,
#36324,#36325),.UNSPECIFIED.,.F.,.F.,(4,3,3,3,3,3,3,3,3,3,3,3,3,4),(-16.6596033343838,
-16.2335874019654,-15.7416605109967,-15.2497336200281,-14.7578067290594,
-14.2658798380908,-13.7739529471221,-13.2820260561535,-12.7900991651849,
-12.2981722742162,-11.8062453832476,-11.3143184922789,-10.8223916013103,
-10.3764180272043),.UNSPECIFIED.);
#1336=B_SPLINE_CURVE_WITH_KNOTS('',3,(#36326,#36327,#36328,#36329,#36330,
#36331,#36332,#36333,#36334,#36335,#36336,#36337,#36338,#36339,#36340,#36341,
#36342,#36343,#36344,#36345,#36346,#36347,#36348,#36349,#36350,#36351,#36352,
#36353,#36354,#36355,#36356,#36357,#36358,#36359,#36360,#36361,#36362,#36363,
#36364,#36365),.UNSPECIFIED.,.F.,.F.,(4,3,3,3,3,3,3,3,3,3,3,3,3,4),(7.40290411470015,
7.87083025549838,8.36275714646703,8.85468403743567,9.34661092840432,9.83853781937297,
10.3304647103416,10.8223916013103,11.3143184922789,11.8062453832476,12.2981722742162,
12.7900991651849,13.2820260561535,13.6860894218797),.UNSPECIFIED.);
#1337=B_SPLINE_CURVE_WITH_KNOTS('',3,(#36370,#36371,#36372,#36373,#36374,
#36375,#36376,#36377,#36378,#36379,#36380,#36381,#36382,#36383,#36384,#36385,
#36386,#36387,#36388,#36389,#36390,#36391,#36392,#36393,#36394,#36395,#36396,
#36397,#36398,#36399,#36400,#36401,#36402,#36403,#36404,#36405,#36406,#36407,
#36408,#36409,#36410,#36411,#36412),.UNSPECIFIED.,.F.,.F.,(4,3,3,3,3,3,
3,3,3,3,3,3,3,3,4),(-22.9427886415634,-22.6286369845578,-22.1367100935892,
-21.6447832026205,-21.1528563116519,-20.6609294206832,-20.1690025297146,
-19.6770756387459,-19.1851487477773,-18.6932218568086,-18.20129496584,-17.7093680748713,
-17.2174411839027,-16.725514292934,-16.6596033343838),.UNSPECIFIED.);
#1338=B_SPLINE_CURVE_WITH_KNOTS('',3,(#36413,#36414,#36415,#36416,#36417,
#36418,#36419,#36420,#36421,#36422,#36423,#36424,#36425,#36426,#36427,#36428,
#36429,#36430,#36431,#36432,#36433,#36434,#36435,#36436,#36437,#36438,#36439,
#36440,#36441,#36442,#36443,#36444,#36445,#36446,#36447,#36448,#36449,#36450,
#36451,#36452,#36453,#36454,#36455),.UNSPECIFIED.,.F.,.F.,(4,3,3,3,3,3,
3,3,3,3,3,3,3,3,4),(13.6860894218797,13.7739529471222,14.2658798380908,
14.7578067290594,15.2497336200281,15.7416605109967,16.2335874019654,16.725514292934,
17.2174411839027,17.7093680748713,18.20129496584,18.6932218568086,19.1851487477773,
19.6770756387459,19.9692747290593),.UNSPECIFIED.);
#1339=B_SPLINE_CURVE_WITH_KNOTS('',3,(#36460,#36461,#36462,#36463,#36464,
#36465,#36466,#36467,#36468,#36469,#36470,#36471,#36472,#36473,#36474,#36475,
#36476,#36477,#36478,#36479,#36480,#36481,#36482,#36483,#36484,#36485,#36486,
#36487,#36488,#36489,#36490,#36491,#36492,#36493,#36494,#36495,#36496,#36497,
#36498,#36499,#36500,#36501,#36502),.UNSPECIFIED.,.F.,.F.,(4,3,3,3,3,3,
3,3,3,3,3,3,3,3,4),(-29.225973948743,-29.0236865671502,-28.5317596761816,
-28.039832785213,-27.5479058942443,-27.0559790032757,-26.564052112307,-26.0721252213384,
-25.5801983303697,-25.0882714394011,-24.5963445484324,-24.1044176574638,
-23.6124907664951,-23.1205638755265,-22.9427886415634),.UNSPECIFIED.);
#1340=B_SPLINE_CURVE_WITH_KNOTS('',3,(#36503,#36504,#36505,#36506,#36507,
#36508,#36509,#36510,#36511,#36512,#36513,#36514,#36515,#36516,#36517,#36518,
#36519,#36520,#36521,#36522,#36523,#36524,#36525,#36526,#36527,#36528,#36529,
#36530,#36531,#36532,#36533,#36534,#36535,#36536,#36537,#36538,#36539,#36540,
#36541,#36542,#36543,#36544,#36545),.UNSPECIFIED.,.F.,.F.,(4,3,3,3,3,3,
3,3,3,3,3,3,3,3,4),(19.9692747290593,20.1690025297146,20.6609294206832,
21.1528563116519,21.6447832026205,22.1367100935892,22.6286369845578,23.1205638755265,
23.6124907664951,24.1044176574638,24.5963445484324,25.0882714394011,25.5801983303697,
26.0721252213384,26.2524600362389),.UNSPECIFIED.);
#1341=B_SPLINE_CURVE_WITH_KNOTS('',3,(#36550,#36551,#36552,#36553,#36554,
#36555,#36556,#36557,#36558,#36559,#36560,#36561,#36562,#36563,#36564,#36565,
#36566,#36567,#36568,#36569,#36570,#36571,#36572,#36573,#36574,#36575,#36576,
#36577,#36578,#36579,#36580,#36581,#36582,#36583,#36584,#36585,#36586,#36587,
#36588,#36589,#36590,#36591,#36592),.UNSPECIFIED.,.F.,.F.,(4,3,3,3,3,3,
3,3,3,3,3,3,3,3,4),(-35.5091592559226,-35.4187361497427,-34.926809258774,
-34.4348823678054,-33.9429554768367,-33.4510285858681,-32.9591016948994,
-32.4671748039308,-31.9752479129621,-31.4833210219935,-30.9913941310248,
-30.4994672400562,-30.0075403490876,-29.5156134581189,-29.225973948743),
 .UNSPECIFIED.);
#1342=B_SPLINE_CURVE_WITH_KNOTS('',3,(#36593,#36594,#36595,#36596,#36597,
#36598,#36599,#36600,#36601,#36602,#36603,#36604,#36605,#36606,#36607,#36608,
#36609,#36610,#36611,#36612,#36613,#36614,#36615,#36616,#36617,#36618,#36619,
#36620,#36621,#36622,#36623,#36624,#36625,#36626,#36627,#36628,#36629,#36630,
#36631,#36632,#36633,#36634,#36635),.UNSPECIFIED.,.F.,.F.,(4,3,3,3,3,3,
3,3,3,3,3,3,3,3,4),(26.2524600362389,26.564052112307,27.0559790032757,27.5479058942443,
28.0398327852129,28.5317596761816,29.0236865671503,29.5156134581189,30.0075403490875,
30.4994672400562,30.9913941310248,31.4833210219935,31.9752479129621,32.4671748039308,
32.5356453434185),.UNSPECIFIED.);
#1343=B_SPLINE_CURVE_WITH_KNOTS('',3,(#36640,#36641,#36642,#36643,#36644,
#36645,#36646,#36647,#36648,#36649,#36650,#36651,#36652,#36653,#36654,#36655,
#36656,#36657,#36658,#36659,#36660,#36661,#36662,#36663,#36664,#36665,#36666,
#36667,#36668,#36669,#36670,#36671,#36672,#36673,#36674,#36675,#36676,#36677,
#36678,#36679),.UNSPECIFIED.,.F.,.F.,(4,3,3,3,3,3,3,3,3,3,3,3,3,4),(-41.7923445631022,
-41.3218588413665,-40.8299319503978,-40.3380050594292,-39.8460781684605,
-39.3541512774919,-38.8622243865232,-38.3702974955546,-37.8783706045859,
-37.3864437136173,-36.8945168226486,-36.40258993168,-35.9106630407113,-35.5091592559226),
 .UNSPECIFIED.);
#1344=B_SPLINE_CURVE_WITH_KNOTS('',3,(#36680,#36681,#36682,#36683,#36684,
#36685,#36686,#36687,#36688,#36689,#36690,#36691,#36692,#36693,#36694,#36695,
#36696,#36697,#36698,#36699,#36700,#36701,#36702,#36703,#36704,#36705,#36706,
#36707,#36708,#36709,#36710,#36711,#36712,#36713,#36714,#36715,#36716,#36717,
#36718,#36719),.UNSPECIFIED.,.F.,.F.,(4,3,3,3,3,3,3,3,3,3,3,3,3,4),(32.5356453434185,
32.9591016948994,33.4510285858681,33.9429554768367,34.4348823678054,34.926809258774,
35.4187361497427,35.9106630407113,36.40258993168,36.8945168226486,37.3864437136173,
37.8783706045859,38.3702974955546,38.8188306505981),.UNSPECIFIED.);
#1345=B_SPLINE_CURVE_WITH_KNOTS('',3,(#36725,#36726,#36727,#36728,#36729),
 .UNSPECIFIED.,.F.,.F.,(4,1,4),(53.4070751110265,53.4285162802594,53.8167918611471),
 .UNSPECIFIED.);
#1346=B_SPLINE_CURVE_WITH_KNOTS('',3,(#36735,#36736,#36737,#36738,#36739,
#36740,#36741,#36742,#36743,#36744,#36745,#36746,#36747,#36748,#36749,#36750),
 .UNSPECIFIED.,.F.,.F.,(4,1,1,1,1,1,1,1,1,1,1,1,1,4),(47.1238898038469,
47.5253935886356,48.0173204796042,48.5092473705729,49.0011742615415,49.4931011525102,
49.9850280434788,50.4769549344475,50.9688818254161,51.4608087163848,51.9527356073534,
52.4446624983221,52.9365893892907,53.4070751110265),.UNSPECIFIED.);
#1347=B_SPLINE_CURVE_WITH_KNOTS('',3,(#36753,#36754,#36755,#36756,#36757,
#36758,#36759,#36760,#36761,#36762,#36763,#36764,#36765,#36766,#36767),
 .UNSPECIFIED.,.F.,.F.,(4,1,1,1,1,1,1,1,1,1,1,1,4),(47.1238898038469,47.167283539772,
47.6592104307407,48.1511373217093,48.6430642126779,49.1349911036466,49.6269179946152,
50.1188448855839,50.6107717765525,51.1026986675212,51.5946255584898,52.0865524494585,
52.5784793404271),.UNSPECIFIED.);
#1348=B_SPLINE_CURVE_WITH_KNOTS('',3,(#36772,#36773,#36774,#36775,#36776,
#36777,#36778,#36779,#36780,#36781,#36782,#36783,#36784,#36785,#36786,#36787,
#36788),.UNSPECIFIED.,.F.,.F.,(4,1,1,1,1,1,1,1,1,1,1,1,1,1,4),(40.8407044966673,
41.1303440060432,41.6222708970118,42.1141977879805,42.6061246789491,43.0980515699178,
43.5899784608864,44.0819053518551,44.5738322428237,45.0657591337924,45.557686024761,
46.0496129157297,46.5415398066983,47.033466697667,47.1238898038469),
 .UNSPECIFIED.);
#1349=B_SPLINE_CURVE_WITH_KNOTS('',3,(#36789,#36790,#36791,#36792,#36793,
#36794,#36795,#36796,#36797,#36798,#36799,#36800,#36801,#36802,#36803,#36804),
 .UNSPECIFIED.,.F.,.F.,(4,1,1,1,1,1,1,1,1,1,1,1,1,4),(40.8407044966673,
41.2641608481482,41.7560877391169,42.2480146300855,42.7399415210542,43.2318684120228,
43.7237953029915,44.2157221939601,44.7076490849288,45.1995759758974,45.6915028668661,
46.1834297578347,46.6753566488034,47.1238898038469),.UNSPECIFIED.);
#1350=B_SPLINE_CURVE_WITH_KNOTS('',3,(#36809,#36810,#36811,#36812,#36813,
#36814,#36815,#36816,#36817,#36818,#36819,#36820,#36821,#36822,#36823,#36824,
#36825),.UNSPECIFIED.,.F.,.F.,(4,1,1,1,1,1,1,1,1,1,1,1,1,1,4),(34.5575191894877,
34.7352944234507,35.2272213144194,35.719148205388,36.2110750963567,36.7030019873253,
37.194928878294,37.6868557692626,38.1787826602313,38.6707095511999,39.1626364421686,
39.6545633331372,40.1464902241059,40.6384171150745,40.8407044966673),
 .UNSPECIFIED.);
#1351=B_SPLINE_CURVE_WITH_KNOTS('',3,(#36826,#36827,#36828,#36829,#36830,
#36831,#36832,#36833,#36834,#36835,#36836,#36837,#36838,#36839,#36840,#36841,
#36842),.UNSPECIFIED.,.F.,.F.,(4,1,1,1,1,1,1,1,1,1,1,1,1,1,4),(34.5575191894877,
34.8691112655558,35.3610381565244,35.8529650474931,36.3448919384617,36.8368188294304,
37.328745720399,37.8206726113677,38.3125995023363,38.804526393305,39.2964532842736,
39.7883801752423,40.2803070662109,40.7722339571796,40.8407044966673),
 .UNSPECIFIED.);
#1352=B_SPLINE_CURVE_WITH_KNOTS('',3,(#36847,#36848,#36849,#36850,#36851,
#36852,#36853,#36854,#36855,#36856,#36857,#36858,#36859,#36860,#36861,#36862,
#36863),.UNSPECIFIED.,.F.,.F.,(4,1,1,1,1,1,1,1,1,1,1,1,1,1,4),(28.2743338823081,
28.3402448408583,28.832171731827,29.3240986227956,29.8160255137643,30.3079524047329,
30.7998792957016,31.2918061866702,31.7837330776389,32.2756599686075,32.7675868595761,
33.2595137505448,33.7514406415134,34.2433675324821,34.5575191894877),
 .UNSPECIFIED.);
#1353=B_SPLINE_CURVE_WITH_KNOTS('',3,(#36864,#36865,#36866,#36867,#36868,
#36869,#36870,#36871,#36872,#36873,#36874,#36875,#36876,#36877,#36878,#36879,
#36880),.UNSPECIFIED.,.F.,.F.,(4,1,1,1,1,1,1,1,1,1,1,1,1,1,4),(28.2743338823081,
28.4740616829634,28.965988573932,29.4579154649007,29.9498423558693,30.441769246838,
30.9336961378066,31.4256230287753,31.9175499197439,32.4094768107125,32.9014037016812,
33.3933305926498,33.8852574836185,34.3771843745871,34.5575191894877),
 .UNSPECIFIED.);
#1354=B_SPLINE_CURVE_WITH_KNOTS('',3,(#36885,#36886,#36887,#36888,#36889,
#36890,#36891,#36892,#36893,#36894,#36895,#36896,#36897,#36898,#36899,#36900),
 .UNSPECIFIED.,.F.,.F.,(4,1,1,1,1,1,1,1,1,1,1,1,1,4),(21.9911485751285,
22.4371221492345,22.9290490402032,23.4209759311718,23.9129028221405,24.4048297131091,
24.8967566040778,25.3886834950464,25.8806103860151,26.3725372769837,26.8644641679524,
27.356391058921,27.8483179498897,28.2743338823081),.UNSPECIFIED.);
#1355=B_SPLINE_CURVE_WITH_KNOTS('',3,(#36901,#36902,#36903,#36904,#36905,
#36906,#36907,#36908,#36909,#36910,#36911,#36912,#36913,#36914,#36915,#36916,
#36917),.UNSPECIFIED.,.F.,.F.,(4,1,1,1,1,1,1,1,1,1,1,1,1,1,4),(21.9911485751285,
22.0790121003709,22.5709389913396,23.0628658823082,23.5547927732769,24.0467196642455,
24.5386465552142,25.0305734461828,25.5225003371515,26.0144272281201,26.5063541190888,
26.9982810100574,27.4902079010261,27.9821347919947,28.2743338823081),
 .UNSPECIFIED.);
#1356=B_SPLINE_CURVE_WITH_KNOTS('',3,(#36922,#36923,#36924,#36925,#36926,
#36927,#36928,#36929,#36930,#36931,#36932,#36933,#36934,#36935,#36936,#36937,
#36938),.UNSPECIFIED.,.F.,.F.,(4,1,1,1,1,1,1,1,1,1,1,1,1,1,4),(15.707963267949,
16.0420725666421,16.5339994576108,17.0259263485794,17.5178532395481,18.0097801305167,
18.5017070214854,18.993633912454,19.4855608034226,19.9774876943913,20.4694145853599,
20.9613414763286,21.4532683672972,21.9451952582659,21.9911485751285),
 .UNSPECIFIED.);
#1357=B_SPLINE_CURVE_WITH_KNOTS('',3,(#36939,#36940,#36941,#36942,#36943,
#36944,#36945,#36946,#36947,#36948,#36949,#36950,#36951,#36952,#36953,#36954),
 .UNSPECIFIED.,.F.,.F.,(4,1,1,1,1,1,1,1,1,1,1,1,1,4),(15.707963267949,16.1758894087472,
16.6678162997158,17.1597431906845,17.6516700816531,18.1435969726218,18.6355238635904,
19.127450754559,19.6193776455277,20.1113045364963,20.603231427465,21.0951583184336,
21.5870852094023,21.9911485751285),.UNSPECIFIED.);
#1358=B_SPLINE_CURVE_WITH_KNOTS('',3,(#37481,#37482,#37483,#37484,#37485,
#37486,#37487,#37488,#37489,#37490,#37491,#37492,#37493,#37494,#37495,#37496,
#37497,#37498,#37499,#37500,#37501,#37502,#37503,#37504,#37505,#37506,#37507,
#37508,#37509,#37510,#37511,#37512,#37513,#37514,#37515,#37516,#37517,#37518,
#37519,#37520,#37521,#37522,#37523,#37524,#37525,#37526,#37527,#37528,#37529,
#37530,#37531,#37532,#37533,#37534,#37535,#37536,#37537,#37538,#37539,#37540,
#37541,#37542,#37543,#37544,#37545,#37546,#37547,#37548,#37549,#37550,#37551,
#37552,#37553,#37554,#37555,#37556,#37557,#37558,#37559,#37560,#37561,#37562,
#37563,#37564,#37565,#37566,#37567,#37568,#37569,#37570,#37571,#37572,#37573,
#37574,#37575,#37576,#37577,#37578,#37579,#37580,#37581,#37582,#37583,#37584,
#37585,#37586,#37587,#37588,#37589,#37590,#37591,#37592,#37593,#37594,#37595,
#37596,#37597,#37598),.UNSPECIFIED.,.F.,.F.,(4,3,3,3,3,3,3,3,3,3,3,3,3,
3,3,3,3,3,3,3,3,3,3,3,3,3,3,3,3,3,3,3,3,3,3,3,3,3,3,4),(0.,0.0681857667088079,
0.0925871972677255,0.160754560978,0.229084940791933,0.297028988213498,0.325731824200965,
0.342177528396621,0.350245710075725,0.417566470176956,0.484648475094958,
0.526651676113238,0.594048569610555,0.661059854099412,0.682534064088732,
0.689876659026608,0.756288907596956,0.822720771296585,0.888378842570404,
0.950859935385141,1.0026277091569,1.01408476217981,1.0221657938941,1.08723429368861,
1.15277237209404,1.2180345613585,1.2826596930891,1.32383090932414,1.34242463013063,
1.34972676639674,1.36500212555917,1.4295571391601,1.49431742045731,1.5286172236547,
1.55554269307663,1.56437072923404,1.62845754216276,1.69224411523009,1.75508079497207,
1.76871584603644),.UNSPECIFIED.);
#1359=B_SPLINE_CURVE_WITH_KNOTS('',3,(#37599,#37600,#37601,#37602,#37603,
#37604,#37605,#37606,#37607,#37608,#37609,#37610,#37611,#37612,#37613,#37614,
#37615,#37616,#37617,#37618,#37619,#37620,#37621,#37622,#37623),
 .UNSPECIFIED.,.F.,.F.,(4,3,3,3,3,3,3,3,4),(38.8188306505981,38.8622243865232,
39.3541512774919,39.8460781684605,40.3380050594292,40.8299319503978,41.3218588413664,
41.8137857323351,42.2020613132229),.UNSPECIFIED.);
#1360=B_SPLINE_CURVE_WITH_KNOTS('',3,(#37625,#37626,#37627,#37628,#37629,
#37630,#37631,#37632,#37633,#37634,#37635,#37636,#37637,#37638,#37639,#37640,
#37641,#37642,#37643,#37644,#37645,#37646,#37647,#37648,#37649,#37650,#37651,
#37652,#37653,#37654,#37655,#37656,#37657,#37658,#37659,#37660,#37661,#37662,
#37663,#37664,#37665,#37666,#37667,#37668,#37669,#37670,#37671,#37672,#37673,
#37674,#37675,#37676,#37677,#37678,#37679,#37680,#37681,#37682,#37683,#37684,
#37685,#37686,#37687,#37688,#37689,#37690,#37691,#37692,#37693,#37694,#37695,
#37696,#37697,#37698,#37699,#37700,#37701,#37702,#37703,#37704,#37705,#37706,
#37707,#37708,#37709,#37710,#37711,#37712,#37713,#37714,#37715,#37716,#37717,
#37718,#37719,#37720,#37721,#37722,#37723,#37724,#37725,#37726,#37727,#37728,
#37729,#37730,#37731,#37732,#37733,#37734,#37735,#37736,#37737,#37738,#37739,
#37740,#37741,#37742),.UNSPECIFIED.,.F.,.F.,(4,3,3,3,3,3,3,3,3,3,3,3,3,
3,3,3,3,3,3,3,3,3,3,3,3,3,3,3,3,3,3,3,3,3,3,3,3,3,3,4),(-1.76871584603644,
-1.7046191062269,-1.68449640386893,-1.62078305031798,-1.57802061157228,
-1.56415526706134,-1.55145880098442,-1.48728260043853,-1.42252268550912,
-1.35794028991274,-1.34735547013984,-1.33863647768557,-1.27868354035241,
-1.21410507385394,-1.1488154291139,-1.0832642762627,-1.02800537889021,-1.01727641030729,
-1.01007836604066,-0.943992267869414,-0.877500202546595,-0.862228686772767,
-0.796068266380696,-0.729641340063069,-0.692925580960443,-0.684965546630163,
-0.676965689034107,-0.610055994476737,-0.542706920162068,-0.475452030986818,
-0.435915267242059,-0.381425858836801,-0.357586742659501,-0.345662846640054,
-0.337975416418596,-0.270932245595006,-0.202736527078763,-0.134396883544413,
-0.0666964856366526,0.),.UNSPECIFIED.);
#1361=B_SPLINE_CURVE_WITH_KNOTS('',3,(#37743,#37744,#37745,#37746,#37747,
#37748,#37749,#37750,#37751,#37752,#37753,#37754,#37755,#37756,#37757),
 .UNSPECIFIED.,.F.,.F.,(4,1,1,1,1,1,1,1,1,1,1,1,4),(10.3764180272043,10.764693608092,
11.2566204990607,11.7485473900293,12.240474280998,12.7324011719666,13.2243280629353,
13.7162549539039,14.2081818448726,14.7001087358412,15.1920356268099,15.6839625177785,
15.707963267949),.UNSPECIFIED.);
#1362=B_SPLINE_CURVE_WITH_KNOTS('',3,(#37763,#37764,#37765,#37766,#37767,
#37768,#37769,#37770,#37771,#37772,#37773,#37774,#37775,#37776,#37777,#37778,
#37779,#37780,#37781,#37782,#37783,#37784,#37785,#37786,#37787,#37788,#37789,
#37790,#37791,#37792,#37793,#37794,#37795,#37796,#37797,#37798,#37799,#37800,
#37801,#37802,#37803,#37804,#37805,#37806,#37807,#37808,#37809,#37810,#37811,
#37812,#37813,#37814,#37815,#37816,#37817,#37818,#37819,#37820,#37821,#37822,
#37823,#37824,#37825,#37826,#37827,#37828,#37829,#37830,#37831,#37832,#37833,
#37834,#37835,#37836,#37837,#37838,#37839,#37840,#37841,#37842,#37843,#37844,
#37845,#37846,#37847,#37848,#37849,#37850,#37851,#37852,#37853,#37854,#37855,
#37856,#37857,#37858,#37859,#37860,#37861,#37862,#37863,#37864,#37865,#37866,
#37867,#37868,#37869,#37870,#37871,#37872,#37873,#37874,#37875,#37876,#37877,
#37878,#37879,#37880),.UNSPECIFIED.,.F.,.F.,(4,3,3,3,3,3,3,3,3,3,3,3,3,
3,3,3,3,3,3,3,3,3,3,3,3,3,3,3,3,3,3,3,3,3,3,3,3,3,3,4),(-1.7649800298231,
-1.69695540332944,-1.67264917116808,-1.60436612704894,-1.55886208432468,
-1.54212438356654,-1.52874434765788,-1.46113379154541,-1.39371142439958,
-1.3268905026446,-1.31426180337642,-1.30254148063391,-1.24033378525489,
-1.17363505650255,-1.10665338574218,-1.03993414154976,-0.984208628543281,
-0.973017916201771,-0.965501098295893,-0.899548822784076,-0.833828509597175,
-0.817032089523831,-0.75098473138995,-0.685204529665416,-0.64999272147509,
-0.642150879902158,-0.634554921790819,-0.569503767261871,-0.504475361186555,
-0.44018015634379,-0.403510064142809,-0.353071306124958,-0.331004349492148,
-0.318701140225958,-0.310509349318208,-0.246725154889164,-0.182546014491394,
-0.118678891385951,-0.0559773875632533,0.),.UNSPECIFIED.);
#1363=B_SPLINE_CURVE_WITH_KNOTS('',3,(#37883,#37884,#37885,#37886,#37887,
#37888,#37889,#37890,#37891,#37892,#37893,#37894),.UNSPECIFIED.,.F.,.F.,
(4,1,1,1,1,1,1,1,1,4),(11.6147305479243,12.1066574388929,12.5985843298616,
13.0905112208302,13.5824381117989,14.0743650027675,14.5662918937362,15.0582187847048,
15.5501456756735,15.707963267949),.UNSPECIFIED.);
#1364=B_SPLINE_CURVE_WITH_KNOTS('',3,(#38268,#38269,#38270,#38271,#38272,
#38273,#38274,#38275,#38276,#38277,#38278,#38279,#38280,#38281,#38282,#38283,
#38284,#38285,#38286,#38287,#38288,#38289,#38290,#38291,#38292,#38293,#38294,
#38295,#38296,#38297,#38298,#38299,#38300,#38301,#38302,#38303,#38304,#38305,
#38306,#38307,#38308,#38309,#38310,#38311,#38312,#38313,#38314,#38315,#38316,
#38317,#38318,#38319,#38320,#38321,#38322,#38323,#38324,#38325,#38326,#38327,
#38328,#38329,#38330,#38331,#38332,#38333,#38334,#38335,#38336,#38337,#38338,
#38339,#38340,#38341,#38342,#38343,#38344,#38345,#38346,#38347,#38348,#38349,
#38350,#38351,#38352,#38353,#38354,#38355,#38356,#38357,#38358,#38359,#38360,
#38361,#38362,#38363,#38364,#38365,#38366,#38367,#38368,#38369,#38370,#38371,
#38372,#38373,#38374,#38375,#38376,#38377,#38378,#38379,#38380,#38381,#38382,
#38383,#38384,#38385),.UNSPECIFIED.,.F.,.F.,(4,3,3,3,3,3,3,3,3,3,3,3,3,
3,3,3,3,3,3,3,3,3,3,3,3,3,3,3,3,3,3,3,3,3,3,3,3,3,3,4),(0.,0.0639852145080714,
0.0841315994229438,0.147534957977308,0.211548544081093,0.275702344548213,
0.302478627892936,0.313393109737379,0.322947639997341,0.387624471507211,
0.452753158889431,0.489912611305994,0.554799697618439,0.59863435069713,
0.636989672140985,0.646993091751658,0.712495556481525,0.778459230466718,
0.844342605144468,0.905476922247968,0.958616291747051,0.969438383973272,
0.97699070665728,1.04256627278548,1.10903071984032,1.17600606522964,1.24274532490853,
1.28666860157458,1.30107863274988,1.30945456030415,1.33059187824063,1.39733368263577,
1.46475749791685,1.50228531440513,1.53103728641692,1.54149218732251,1.60963039313057,
1.6779332296461,1.74577594078118,1.76498002982309),.UNSPECIFIED.);
#1365=B_SPLINE_CURVE_WITH_KNOTS('',3,(#38386,#38387,#38388,#38389,#38390,
#38391,#38392,#38393,#38394,#38395,#38396,#38397,#38398,#38399,#38400,#38401,
#38402,#38403,#38404),.UNSPECIFIED.,.F.,.F.,(4,3,3,3,3,3,4),(-44.2734201871783,
-43.7814932962097,-43.289566405241,-42.7976395142724,-42.3057126233038,
-41.8137857323351,-41.7923445631022),.UNSPECIFIED.);
#1366=CYLINDRICAL_SURFACE('',#15257,15.);
#1367=CYLINDRICAL_SURFACE('',#15269,7.15);
#1368=CYLINDRICAL_SURFACE('',#15276,15.);
#1369=CYLINDRICAL_SURFACE('',#15286,7.15);
#1370=CYLINDRICAL_SURFACE('',#15290,9.05);
#1371=CYLINDRICAL_SURFACE('',#15304,6.05);
#1372=CYLINDRICAL_SURFACE('',#15308,6.05);
#1373=CYLINDRICAL_SURFACE('',#15312,6.05);
#1374=CYLINDRICAL_SURFACE('',#15316,6.05);
#1375=CYLINDRICAL_SURFACE('',#15332,62.5);
#1376=CYLINDRICAL_SURFACE('',#15351,62.5);
#1377=CYLINDRICAL_SURFACE('',#15367,2.);
#1378=CYLINDRICAL_SURFACE('',#15372,2.);
#1379=CYLINDRICAL_SURFACE('',#15378,2.);
#1380=CYLINDRICAL_SURFACE('',#15379,2.);
#1381=CYLINDRICAL_SURFACE('',#15380,14.);
#1382=CYLINDRICAL_SURFACE('',#15385,2.);
#1383=CYLINDRICAL_SURFACE('',#15390,2.);
#1384=CYLINDRICAL_SURFACE('',#15392,14.);
#1385=CYLINDRICAL_SURFACE('',#15396,2.);
#1386=CYLINDRICAL_SURFACE('',#15400,2.);
#1387=CYLINDRICAL_SURFACE('',#15406,50.8);
#1388=CYLINDRICAL_SURFACE('',#15407,2.);
#1389=CYLINDRICAL_SURFACE('',#15413,2.);
#1390=CYLINDRICAL_SURFACE('',#15420,2.);
#1391=CYLINDRICAL_SURFACE('',#15421,2.);
#1392=CYLINDRICAL_SURFACE('',#15423,2.);
#1393=CYLINDRICAL_SURFACE('',#15429,2.);
#1394=CYLINDRICAL_SURFACE('',#15431,2.);
#1395=CYLINDRICAL_SURFACE('',#15437,2.);
#1396=CYLINDRICAL_SURFACE('',#15439,2.);
#1397=CYLINDRICAL_SURFACE('',#15445,2.);
#1398=CYLINDRICAL_SURFACE('',#15450,2.);
#1399=CYLINDRICAL_SURFACE('',#15455,2.);
#1400=CYLINDRICAL_SURFACE('',#15459,28.);
#1401=CYLINDRICAL_SURFACE('',#15460,28.);
#1402=CYLINDRICAL_SURFACE('',#15465,50.);
#1403=CYLINDRICAL_SURFACE('',#15472,9.05);
#1404=CYLINDRICAL_SURFACE('',#15477,23.525);
#1405=CYLINDRICAL_SURFACE('',#15482,27.505);
#1406=CYLINDRICAL_SURFACE('',#15486,26.);
#1407=CYLINDRICAL_SURFACE('',#15490,28.);
#1408=CYLINDRICAL_SURFACE('',#15491,28.);
#1409=CYLINDRICAL_SURFACE('',#15501,13.);
#1410=CYLINDRICAL_SURFACE('',#15511,19.);
#1411=CYLINDRICAL_SURFACE('',#15520,2.);
#1412=CYLINDRICAL_SURFACE('',#15523,6.05);
#1413=CYLINDRICAL_SURFACE('',#15531,2.);
#1414=CYLINDRICAL_SURFACE('',#15534,6.05);
#1415=CYLINDRICAL_SURFACE('',#15542,6.05);
#1416=CYLINDRICAL_SURFACE('',#15550,2.);
#1417=CYLINDRICAL_SURFACE('',#15553,6.05);
#1418=CYLINDRICAL_SURFACE('',#15558,2.);
#1419=CYLINDRICAL_SURFACE('',#15585,5.05000000000001);
#1420=CYLINDRICAL_SURFACE('',#15589,5.04999999999999);
#1421=CYLINDRICAL_SURFACE('',#15593,5.04999999999999);
#1422=CYLINDRICAL_SURFACE('',#15597,5.05000000000001);
#1423=CYLINDRICAL_SURFACE('',#15601,9.49999999999999);
#1424=CYLINDRICAL_SURFACE('',#15604,6.);
#1425=CYLINDRICAL_SURFACE('',#15606,2.);
#1426=CYLINDRICAL_SURFACE('',#15612,2.);
#1427=CYLINDRICAL_SURFACE('',#15614,2.);
#1428=CYLINDRICAL_SURFACE('',#15615,2.);
#1429=CYLINDRICAL_SURFACE('',#15619,2.);
#1430=CYLINDRICAL_SURFACE('',#15624,2.);
#1431=CYLINDRICAL_SURFACE('',#15626,2.);
#1432=CYLINDRICAL_SURFACE('',#15633,2.);
#1433=CYLINDRICAL_SURFACE('',#15634,2.);
#1434=CYLINDRICAL_SURFACE('',#15640,2.);
#1435=CYLINDRICAL_SURFACE('',#15641,2.);
#1436=CYLINDRICAL_SURFACE('',#15658,43.05);
#1437=CYLINDRICAL_SURFACE('',#15663,2.);
#1438=CYLINDRICAL_SURFACE('',#15681,28.);
#1439=CYLINDRICAL_SURFACE('',#15700,2.);
#1440=CYLINDRICAL_SURFACE('',#15706,28.);
#1441=CYLINDRICAL_SURFACE('',#15714,2.);
#1442=CYLINDRICAL_SURFACE('',#15728,2.);
#1443=CYLINDRICAL_SURFACE('',#15729,28.);
#1444=CYLINDRICAL_SURFACE('',#15732,28.);
#1445=CYLINDRICAL_SURFACE('',#15733,2.);
#1446=CYLINDRICAL_SURFACE('',#15735,2.);
#1447=CYLINDRICAL_SURFACE('',#15740,2.);
#1448=CYLINDRICAL_SURFACE('',#15741,2.);
#1449=CYLINDRICAL_SURFACE('',#15743,10.);
#1450=CYLINDRICAL_SURFACE('',#15758,2.);
#1451=CYLINDRICAL_SURFACE('',#15761,2.);
#1452=CYLINDRICAL_SURFACE('',#15765,2.);
#1453=CYLINDRICAL_SURFACE('',#15767,2.);
#1454=CYLINDRICAL_SURFACE('',#15768,10.);
#1455=CYLINDRICAL_SURFACE('',#15773,2.);
#1456=CYLINDRICAL_SURFACE('',#15774,6.5);
#1457=CYLINDRICAL_SURFACE('',#15775,6.5);
#1458=CYLINDRICAL_SURFACE('',#15777,6.5);
#1459=CYLINDRICAL_SURFACE('',#15778,6.5);
#1460=CYLINDRICAL_SURFACE('',#15779,10.);
#1461=CYLINDRICAL_SURFACE('',#15781,10.);
#1462=CYLINDRICAL_SURFACE('',#15792,16.6);
#1463=CYLINDRICAL_SURFACE('',#15796,16.505);
#1464=CYLINDRICAL_SURFACE('',#15804,48.);
#1465=CYLINDRICAL_SURFACE('',#15822,48.);
#1466=CYLINDRICAL_SURFACE('',#15823,20.);
#1467=CYLINDRICAL_SURFACE('',#15848,12.51);
#1468=CYLINDRICAL_SURFACE('',#15865,5.);
#1469=CYLINDRICAL_SURFACE('',#15867,8.51);
#1470=CYLINDRICAL_SURFACE('',#15870,5.);
#1471=CYLINDRICAL_SURFACE('',#15872,8.51);
#1472=CYLINDRICAL_SURFACE('',#15875,5.);
#1473=CYLINDRICAL_SURFACE('',#15877,8.51);
#1474=CYLINDRICAL_SURFACE('',#15880,5.);
#1475=CYLINDRICAL_SURFACE('',#15882,8.51);
#1476=CYLINDRICAL_SURFACE('',#15885,5.);
#1477=CYLINDRICAL_SURFACE('',#15887,8.51);
#1478=CYLINDRICAL_SURFACE('',#15890,5.);
#1479=CYLINDRICAL_SURFACE('',#15892,8.51);
#1480=CYLINDRICAL_SURFACE('',#15895,5.);
#1481=CYLINDRICAL_SURFACE('',#15897,8.51);
#1482=CYLINDRICAL_SURFACE('',#15900,42.5);
#1483=CYLINDRICAL_SURFACE('',#15930,33.);
#1484=CYLINDRICAL_SURFACE('',#15933,23.);
#1485=CYLINDRICAL_SURFACE('',#15936,33.);
#1486=CYLINDRICAL_SURFACE('',#15939,23.);
#1487=CYLINDRICAL_SURFACE('',#15942,15.5);
#1488=CYLINDRICAL_SURFACE('',#15947,43.);
#1489=CYLINDRICAL_SURFACE('',#15993,11.1);
#1490=CYLINDRICAL_SURFACE('',#16103,3.35);
#1491=CYLINDRICAL_SURFACE('',#16139,15.);
#1492=CYLINDRICAL_SURFACE('',#16143,14.);
#1493=CYLINDRICAL_SURFACE('',#16147,12.5);
#1494=CYLINDRICAL_SURFACE('',#16183,27.5);
#1495=CYLINDRICAL_SURFACE('',#16199,15.);
#1496=CYLINDRICAL_SURFACE('',#16205,12.5);
#1497=CYLINDRICAL_SURFACE('',#16212,15.6);
#1498=CYLINDRICAL_SURFACE('',#16214,13.5);
#1499=CYLINDRICAL_SURFACE('',#16219,16.5);
#1500=CYLINDRICAL_SURFACE('',#16223,13.5);
#1501=CYLINDRICAL_SURFACE('',#16226,15.6);
#1502=CYLINDRICAL_SURFACE('',#16236,20.5);
#1503=CYLINDRICAL_SURFACE('',#16246,15.);
#1504=CYLINDRICAL_SURFACE('',#16250,23.52);
#1505=CYLINDRICAL_SURFACE('',#16258,4.);
#1506=CYLINDRICAL_SURFACE('',#16262,1.);
#1507=CYLINDRICAL_SURFACE('',#16267,4.);
#1508=CYLINDRICAL_SURFACE('',#16275,8.5);
#1509=CYLINDRICAL_SURFACE('',#16280,5.);
#1510=CYLINDRICAL_SURFACE('',#16287,11.);
#1511=CYLINDRICAL_SURFACE('',#16291,9.);
#1512=CYLINDRICAL_SURFACE('',#16301,2.);
#1513=CYLINDRICAL_SURFACE('',#16324,41.);
#1514=CYLINDRICAL_SURFACE('',#16326,10.5);
#1515=CYLINDRICAL_SURFACE('',#16328,22.);
#1516=CYLINDRICAL_SURFACE('',#16330,10.5);
#1517=CYLINDRICAL_SURFACE('',#16332,22.);
#1518=CYLINDRICAL_SURFACE('',#16334,10.5);
#1519=CYLINDRICAL_SURFACE('',#16336,22.);
#1520=CYLINDRICAL_SURFACE('',#16338,10.5);
#1521=CYLINDRICAL_SURFACE('',#16340,22.);
#1522=CYLINDRICAL_SURFACE('',#16342,10.5);
#1523=CYLINDRICAL_SURFACE('',#16344,22.);
#1524=CYLINDRICAL_SURFACE('',#16346,10.5);
#1525=CYLINDRICAL_SURFACE('',#16348,22.);
#1526=CYLINDRICAL_SURFACE('',#16350,10.5);
#1527=CYLINDRICAL_SURFACE('',#16355,22.);
#1528=CYLINDRICAL_SURFACE('',#16358,5.91675);
#1529=CYLINDRICAL_SURFACE('',#16360,5.91675);
#1530=CYLINDRICAL_SURFACE('',#16361,5.91675);
#1531=CYLINDRICAL_SURFACE('',#16362,5.91675);
#1532=CYLINDRICAL_SURFACE('',#16363,5.91675);
#1533=CYLINDRICAL_SURFACE('',#16364,5.91675);
#1534=CYLINDRICAL_SURFACE('',#16365,5.91675);
#1535=CYLINDRICAL_SURFACE('',#16366,5.91675);
#1536=CYLINDRICAL_SURFACE('',#16367,5.91675);
#1537=CYLINDRICAL_SURFACE('',#16368,5.91675);
#1538=CYLINDRICAL_SURFACE('',#16369,5.91675);
#1539=CYLINDRICAL_SURFACE('',#16370,5.91675);
#1540=CYLINDRICAL_SURFACE('',#16371,5.91675);
#1541=CYLINDRICAL_SURFACE('',#16372,5.91675);
#1542=CYLINDRICAL_SURFACE('',#16373,5.91675);
#1543=CYLINDRICAL_SURFACE('',#16374,5.91675);
#1544=CYLINDRICAL_SURFACE('',#16375,5.91675);
#1545=CYLINDRICAL_SURFACE('',#16376,5.91675);
#1546=CYLINDRICAL_SURFACE('',#16377,5.91675);
#1547=CYLINDRICAL_SURFACE('',#16378,5.91675);
#1548=CYLINDRICAL_SURFACE('',#16379,5.91675);
#1549=CYLINDRICAL_SURFACE('',#16380,5.91675);
#1550=CYLINDRICAL_SURFACE('',#16381,5.91675);
#1551=CYLINDRICAL_SURFACE('',#16382,5.91675);
#1552=CYLINDRICAL_SURFACE('',#16383,5.91675);
#1553=CYLINDRICAL_SURFACE('',#16384,5.91675);
#1554=CYLINDRICAL_SURFACE('',#16385,5.91675);
#1555=CYLINDRICAL_SURFACE('',#16386,5.91675);
#1556=CYLINDRICAL_SURFACE('',#16387,5.91675);
#1557=CYLINDRICAL_SURFACE('',#16388,5.91675);
#1558=CYLINDRICAL_SURFACE('',#16389,5.91675);
#1559=CYLINDRICAL_SURFACE('',#16390,5.91675);
#1560=CYLINDRICAL_SURFACE('',#16391,5.91675);
#1561=CYLINDRICAL_SURFACE('',#16392,5.91675);
#1562=CYLINDRICAL_SURFACE('',#16393,4.91825);
#1563=CYLINDRICAL_SURFACE('',#16395,4.91825);
#1564=CYLINDRICAL_SURFACE('',#16396,4.91825);
#1565=CYLINDRICAL_SURFACE('',#16397,4.91825);
#1566=CYLINDRICAL_SURFACE('',#16398,4.91825);
#1567=CYLINDRICAL_SURFACE('',#16399,4.91825);
#1568=CYLINDRICAL_SURFACE('',#16400,4.91825);
#1569=CYLINDRICAL_SURFACE('',#16401,4.91825);
#1570=CYLINDRICAL_SURFACE('',#16402,4.91825);
#1571=CYLINDRICAL_SURFACE('',#16403,4.91825);
#1572=CYLINDRICAL_SURFACE('',#16404,4.91825);
#1573=CYLINDRICAL_SURFACE('',#16405,4.91825);
#1574=CYLINDRICAL_SURFACE('',#16406,4.91825);
#1575=CYLINDRICAL_SURFACE('',#16407,4.91825);
#1576=CYLINDRICAL_SURFACE('',#16408,4.91825);
#1577=CYLINDRICAL_SURFACE('',#16409,4.91825);
#1578=CYLINDRICAL_SURFACE('',#16410,4.91825);
#1579=CYLINDRICAL_SURFACE('',#16411,4.91825);
#1580=CYLINDRICAL_SURFACE('',#16412,4.91825);
#1581=CYLINDRICAL_SURFACE('',#16413,4.91825);
#1582=CYLINDRICAL_SURFACE('',#16414,4.91825);
#1583=CYLINDRICAL_SURFACE('',#16415,4.91825);
#1584=CYLINDRICAL_SURFACE('',#16416,4.91825);
#1585=CYLINDRICAL_SURFACE('',#16417,4.91825);
#1586=CYLINDRICAL_SURFACE('',#16418,4.91825);
#1587=CYLINDRICAL_SURFACE('',#16419,4.91825);
#1588=CYLINDRICAL_SURFACE('',#16420,4.91825);
#1589=CYLINDRICAL_SURFACE('',#16421,4.91825);
#1590=CYLINDRICAL_SURFACE('',#16422,4.91825);
#1591=CYLINDRICAL_SURFACE('',#16423,4.91825);
#1592=CYLINDRICAL_SURFACE('',#16424,4.91825);
#1593=CYLINDRICAL_SURFACE('',#16425,4.91825);
#1594=CYLINDRICAL_SURFACE('',#16426,4.91825);
#1595=CYLINDRICAL_SURFACE('',#16427,4.91825);
#1596=CYLINDRICAL_SURFACE('',#16432,4.91825);
#1597=CYLINDRICAL_SURFACE('',#16661,5.91675);
#1598=CYLINDRICAL_SURFACE('',#16665,9.);
#1599=CYLINDRICAL_SURFACE('',#16671,8.925);
#1600=CYLINDRICAL_SURFACE('',#16673,8.925);
#1601=CYLINDRICAL_SURFACE('',#16674,8.925);
#1602=CYLINDRICAL_SURFACE('',#16675,8.925);
#1603=CYLINDRICAL_SURFACE('',#16676,8.925);
#1604=CYLINDRICAL_SURFACE('',#16677,8.925);
#1605=CYLINDRICAL_SURFACE('',#16678,8.925);
#1606=CYLINDRICAL_SURFACE('',#16679,8.0685);
#1607=CYLINDRICAL_SURFACE('',#16681,8.0685);
#1608=CYLINDRICAL_SURFACE('',#16683,8.0685);
#1609=CYLINDRICAL_SURFACE('',#16684,8.0685);
#1610=CYLINDRICAL_SURFACE('',#16685,8.0685);
#1611=CYLINDRICAL_SURFACE('',#16686,8.0685);
#1612=CYLINDRICAL_SURFACE('',#16687,8.0685);
#1613=CYLINDRICAL_SURFACE('',#16723,8.0685);
#1614=CYLINDRICAL_SURFACE('',#16739,12.5);
#1615=CYLINDRICAL_SURFACE('',#16743,8.925);
#1616=CYLINDRICAL_SURFACE('',#16744,8.);
#1617=FACE_OUTER_BOUND('',#2504,.T.);
#1618=FACE_OUTER_BOUND('',#2505,.T.);
#1619=FACE_OUTER_BOUND('',#2506,.T.);
#1620=FACE_OUTER_BOUND('',#2508,.T.);
#1621=FACE_OUTER_BOUND('',#2509,.T.);
#1622=FACE_OUTER_BOUND('',#2511,.T.);
#1623=FACE_OUTER_BOUND('',#2512,.T.);
#1624=FACE_OUTER_BOUND('',#2513,.T.);
#1625=FACE_OUTER_BOUND('',#2515,.T.);
#1626=FACE_OUTER_BOUND('',#2516,.T.);
#1627=FACE_OUTER_BOUND('',#2517,.T.);
#1628=FACE_OUTER_BOUND('',#2519,.T.);
#1629=FACE_OUTER_BOUND('',#2520,.T.);
#1630=FACE_OUTER_BOUND('',#2521,.T.);
#1631=FACE_OUTER_BOUND('',#2522,.T.);
#1632=FACE_OUTER_BOUND('',#2523,.T.);
#1633=FACE_OUTER_BOUND('',#2529,.T.);
#1634=FACE_OUTER_BOUND('',#2530,.T.);
#1635=FACE_OUTER_BOUND('',#2531,.T.);
#1636=FACE_OUTER_BOUND('',#2532,.T.);
#1637=FACE_OUTER_BOUND('',#2533,.T.);
#1638=FACE_OUTER_BOUND('',#2534,.T.);
#1639=FACE_OUTER_BOUND('',#2535,.T.);
#1640=FACE_OUTER_BOUND('',#2536,.T.);
#1641=FACE_OUTER_BOUND('',#2537,.T.);
#1642=FACE_OUTER_BOUND('',#2538,.T.);
#1643=FACE_OUTER_BOUND('',#2539,.T.);
#1644=FACE_OUTER_BOUND('',#2540,.T.);
#1645=FACE_OUTER_BOUND('',#2541,.T.);
#1646=FACE_OUTER_BOUND('',#2542,.T.);
#1647=FACE_OUTER_BOUND('',#2543,.T.);
#1648=FACE_OUTER_BOUND('',#2544,.T.);
#1649=FACE_OUTER_BOUND('',#2545,.T.);
#1650=FACE_OUTER_BOUND('',#2546,.T.);
#1651=FACE_OUTER_BOUND('',#2547,.T.);
#1652=FACE_OUTER_BOUND('',#2548,.T.);
#1653=FACE_OUTER_BOUND('',#2549,.T.);
#1654=FACE_OUTER_BOUND('',#2550,.T.);
#1655=FACE_OUTER_BOUND('',#2551,.T.);
#1656=FACE_OUTER_BOUND('',#2552,.T.);
#1657=FACE_OUTER_BOUND('',#2553,.T.);
#1658=FACE_OUTER_BOUND('',#2554,.T.);
#1659=FACE_OUTER_BOUND('',#2555,.T.);
#1660=FACE_OUTER_BOUND('',#2559,.T.);
#1661=FACE_OUTER_BOUND('',#2560,.T.);
#1662=FACE_OUTER_BOUND('',#2561,.T.);
#1663=FACE_OUTER_BOUND('',#2562,.T.);
#1664=FACE_OUTER_BOUND('',#2563,.T.);
#1665=FACE_OUTER_BOUND('',#2564,.T.);
#1666=FACE_OUTER_BOUND('',#2565,.T.);
#1667=FACE_OUTER_BOUND('',#2566,.T.);
#1668=FACE_OUTER_BOUND('',#2567,.T.);
#1669=FACE_OUTER_BOUND('',#2568,.T.);
#1670=FACE_OUTER_BOUND('',#2569,.T.);
#1671=FACE_OUTER_BOUND('',#2570,.T.);
#1672=FACE_OUTER_BOUND('',#2571,.T.);
#1673=FACE_OUTER_BOUND('',#2572,.T.);
#1674=FACE_OUTER_BOUND('',#2573,.T.);
#1675=FACE_OUTER_BOUND('',#2574,.T.);
#1676=FACE_OUTER_BOUND('',#2575,.T.);
#1677=FACE_OUTER_BOUND('',#2576,.T.);
#1678=FACE_OUTER_BOUND('',#2577,.T.);
#1679=FACE_OUTER_BOUND('',#2578,.T.);
#1680=FACE_OUTER_BOUND('',#2579,.T.);
#1681=FACE_OUTER_BOUND('',#2580,.T.);
#1682=FACE_OUTER_BOUND('',#2581,.T.);
#1683=FACE_OUTER_BOUND('',#2582,.T.);
#1684=FACE_OUTER_BOUND('',#2583,.T.);
#1685=FACE_OUTER_BOUND('',#2584,.T.);
#1686=FACE_OUTER_BOUND('',#2585,.T.);
#1687=FACE_OUTER_BOUND('',#2586,.T.);
#1688=FACE_OUTER_BOUND('',#2587,.T.);
#1689=FACE_OUTER_BOUND('',#2588,.T.);
#1690=FACE_OUTER_BOUND('',#2589,.T.);
#1691=FACE_OUTER_BOUND('',#2590,.T.);
#1692=FACE_OUTER_BOUND('',#2591,.T.);
#1693=FACE_OUTER_BOUND('',#2592,.T.);
#1694=FACE_OUTER_BOUND('',#2593,.T.);
#1695=FACE_OUTER_BOUND('',#2594,.T.);
#1696=FACE_OUTER_BOUND('',#2595,.T.);
#1697=FACE_OUTER_BOUND('',#2596,.T.);
#1698=FACE_OUTER_BOUND('',#2597,.T.);
#1699=FACE_OUTER_BOUND('',#2598,.T.);
#1700=FACE_OUTER_BOUND('',#2599,.T.);
#1701=FACE_OUTER_BOUND('',#2600,.T.);
#1702=FACE_OUTER_BOUND('',#2601,.T.);
#1703=FACE_OUTER_BOUND('',#2602,.T.);
#1704=FACE_OUTER_BOUND('',#2603,.T.);
#1705=FACE_OUTER_BOUND('',#2604,.T.);
#1706=FACE_OUTER_BOUND('',#2605,.T.);
#1707=FACE_OUTER_BOUND('',#2606,.T.);
#1708=FACE_OUTER_BOUND('',#2607,.T.);
#1709=FACE_OUTER_BOUND('',#2608,.T.);
#1710=FACE_OUTER_BOUND('',#2609,.T.);
#1711=FACE_OUTER_BOUND('',#2610,.T.);
#1712=FACE_OUTER_BOUND('',#2611,.T.);
#1713=FACE_OUTER_BOUND('',#2614,.T.);
#1714=FACE_OUTER_BOUND('',#2615,.T.);
#1715=FACE_OUTER_BOUND('',#2616,.T.);
#1716=FACE_OUTER_BOUND('',#2617,.T.);
#1717=FACE_OUTER_BOUND('',#2618,.T.);
#1718=FACE_OUTER_BOUND('',#2619,.T.);
#1719=FACE_OUTER_BOUND('',#2620,.T.);
#1720=FACE_OUTER_BOUND('',#2621,.T.);
#1721=FACE_OUTER_BOUND('',#2622,.T.);
#1722=FACE_OUTER_BOUND('',#2623,.T.);
#1723=FACE_OUTER_BOUND('',#2624,.T.);
#1724=FACE_OUTER_BOUND('',#2625,.T.);
#1725=FACE_OUTER_BOUND('',#2626,.T.);
#1726=FACE_OUTER_BOUND('',#2627,.T.);
#1727=FACE_OUTER_BOUND('',#2628,.T.);
#1728=FACE_OUTER_BOUND('',#2630,.T.);
#1729=FACE_OUTER_BOUND('',#2631,.T.);
#1730=FACE_OUTER_BOUND('',#2633,.T.);
#1731=FACE_OUTER_BOUND('',#2634,.T.);
#1732=FACE_OUTER_BOUND('',#2636,.T.);
#1733=FACE_OUTER_BOUND('',#2638,.T.);
#1734=FACE_OUTER_BOUND('',#2639,.T.);
#1735=FACE_OUTER_BOUND('',#2640,.T.);
#1736=FACE_OUTER_BOUND('',#2641,.T.);
#1737=FACE_OUTER_BOUND('',#2642,.T.);
#1738=FACE_OUTER_BOUND('',#2643,.T.);
#1739=FACE_OUTER_BOUND('',#2645,.T.);
#1740=FACE_OUTER_BOUND('',#2646,.T.);
#1741=FACE_OUTER_BOUND('',#2647,.T.);
#1742=FACE_OUTER_BOUND('',#2649,.T.);
#1743=FACE_OUTER_BOUND('',#2650,.T.);
#1744=FACE_OUTER_BOUND('',#2651,.T.);
#1745=FACE_OUTER_BOUND('',#2652,.T.);
#1746=FACE_OUTER_BOUND('',#2653,.T.);
#1747=FACE_OUTER_BOUND('',#2654,.T.);
#1748=FACE_OUTER_BOUND('',#2655,.T.);
#1749=FACE_OUTER_BOUND('',#2656,.T.);
#1750=FACE_OUTER_BOUND('',#2657,.T.);
#1751=FACE_OUTER_BOUND('',#2658,.T.);
#1752=FACE_OUTER_BOUND('',#2659,.T.);
#1753=FACE_OUTER_BOUND('',#2660,.T.);
#1754=FACE_OUTER_BOUND('',#2661,.T.);
#1755=FACE_OUTER_BOUND('',#2662,.T.);
#1756=FACE_OUTER_BOUND('',#2663,.T.);
#1757=FACE_OUTER_BOUND('',#2664,.T.);
#1758=FACE_OUTER_BOUND('',#2665,.T.);
#1759=FACE_OUTER_BOUND('',#2666,.T.);
#1760=FACE_OUTER_BOUND('',#2667,.T.);
#1761=FACE_OUTER_BOUND('',#2668,.T.);
#1762=FACE_OUTER_BOUND('',#2669,.T.);
#1763=FACE_OUTER_BOUND('',#2670,.T.);
#1764=FACE_OUTER_BOUND('',#2671,.T.);
#1765=FACE_OUTER_BOUND('',#2672,.T.);
#1766=FACE_OUTER_BOUND('',#2673,.T.);
#1767=FACE_OUTER_BOUND('',#2674,.T.);
#1768=FACE_OUTER_BOUND('',#2675,.T.);
#1769=FACE_OUTER_BOUND('',#2676,.T.);
#1770=FACE_OUTER_BOUND('',#2677,.T.);
#1771=FACE_OUTER_BOUND('',#2678,.T.);
#1772=FACE_OUTER_BOUND('',#2679,.T.);
#1773=FACE_OUTER_BOUND('',#2680,.T.);
#1774=FACE_OUTER_BOUND('',#2681,.T.);
#1775=FACE_OUTER_BOUND('',#2682,.T.);
#1776=FACE_OUTER_BOUND('',#2683,.T.);
#1777=FACE_OUTER_BOUND('',#2684,.T.);
#1778=FACE_OUTER_BOUND('',#2685,.T.);
#1779=FACE_OUTER_BOUND('',#2686,.T.);
#1780=FACE_OUTER_BOUND('',#2687,.T.);
#1781=FACE_OUTER_BOUND('',#2688,.T.);
#1782=FACE_OUTER_BOUND('',#2689,.T.);
#1783=FACE_OUTER_BOUND('',#2690,.T.);
#1784=FACE_OUTER_BOUND('',#2691,.T.);
#1785=FACE_OUTER_BOUND('',#2692,.T.);
#1786=FACE_OUTER_BOUND('',#2693,.T.);
#1787=FACE_OUTER_BOUND('',#2694,.T.);
#1788=FACE_OUTER_BOUND('',#2695,.T.);
#1789=FACE_OUTER_BOUND('',#2696,.T.);
#1790=FACE_OUTER_BOUND('',#2697,.T.);
#1791=FACE_OUTER_BOUND('',#2698,.T.);
#1792=FACE_OUTER_BOUND('',#2699,.T.);
#1793=FACE_OUTER_BOUND('',#2700,.T.);
#1794=FACE_OUTER_BOUND('',#2701,.T.);
#1795=FACE_OUTER_BOUND('',#2702,.T.);
#1796=FACE_OUTER_BOUND('',#2703,.T.);
#1797=FACE_OUTER_BOUND('',#2704,.T.);
#1798=FACE_OUTER_BOUND('',#2705,.T.);
#1799=FACE_OUTER_BOUND('',#2706,.T.);
#1800=FACE_OUTER_BOUND('',#2707,.T.);
#1801=FACE_OUTER_BOUND('',#2708,.T.);
#1802=FACE_OUTER_BOUND('',#2714,.T.);
#1803=FACE_OUTER_BOUND('',#2715,.T.);
#1804=FACE_OUTER_BOUND('',#2716,.T.);
#1805=FACE_OUTER_BOUND('',#2717,.T.);
#1806=FACE_OUTER_BOUND('',#2718,.T.);
#1807=FACE_OUTER_BOUND('',#2719,.T.);
#1808=FACE_OUTER_BOUND('',#2720,.T.);
#1809=FACE_OUTER_BOUND('',#2721,.T.);
#1810=FACE_OUTER_BOUND('',#2722,.T.);
#1811=FACE_OUTER_BOUND('',#2723,.T.);
#1812=FACE_OUTER_BOUND('',#2724,.T.);
#1813=FACE_OUTER_BOUND('',#2725,.T.);
#1814=FACE_OUTER_BOUND('',#2726,.T.);
#1815=FACE_OUTER_BOUND('',#2727,.T.);
#1816=FACE_OUTER_BOUND('',#2728,.T.);
#1817=FACE_OUTER_BOUND('',#2729,.T.);
#1818=FACE_OUTER_BOUND('',#2730,.T.);
#1819=FACE_OUTER_BOUND('',#2731,.T.);
#1820=FACE_OUTER_BOUND('',#2732,.T.);
#1821=FACE_OUTER_BOUND('',#2733,.T.);
#1822=FACE_OUTER_BOUND('',#2734,.T.);
#1823=FACE_OUTER_BOUND('',#2735,.T.);
#1824=FACE_OUTER_BOUND('',#2736,.T.);
#1825=FACE_OUTER_BOUND('',#2737,.T.);
#1826=FACE_OUTER_BOUND('',#2738,.T.);
#1827=FACE_OUTER_BOUND('',#2739,.T.);
#1828=FACE_OUTER_BOUND('',#2740,.T.);
#1829=FACE_OUTER_BOUND('',#2741,.T.);
#1830=FACE_OUTER_BOUND('',#2742,.T.);
#1831=FACE_OUTER_BOUND('',#2743,.T.);
#1832=FACE_OUTER_BOUND('',#2744,.T.);
#1833=FACE_OUTER_BOUND('',#2745,.T.);
#1834=FACE_OUTER_BOUND('',#2746,.T.);
#1835=FACE_OUTER_BOUND('',#2752,.T.);
#1836=FACE_OUTER_BOUND('',#2753,.T.);
#1837=FACE_OUTER_BOUND('',#2754,.T.);
#1838=FACE_OUTER_BOUND('',#2755,.T.);
#1839=FACE_OUTER_BOUND('',#2756,.T.);
#1840=FACE_OUTER_BOUND('',#2757,.T.);
#1841=FACE_OUTER_BOUND('',#2758,.T.);
#1842=FACE_OUTER_BOUND('',#2759,.T.);
#1843=FACE_OUTER_BOUND('',#2763,.T.);
#1844=FACE_OUTER_BOUND('',#2764,.T.);
#1845=FACE_OUTER_BOUND('',#2766,.T.);
#1846=FACE_OUTER_BOUND('',#2767,.T.);
#1847=FACE_OUTER_BOUND('',#2768,.T.);
#1848=FACE_OUTER_BOUND('',#2769,.T.);
#1849=FACE_OUTER_BOUND('',#2771,.T.);
#1850=FACE_OUTER_BOUND('',#2772,.T.);
#1851=FACE_OUTER_BOUND('',#2774,.T.);
#1852=FACE_OUTER_BOUND('',#2775,.T.);
#1853=FACE_OUTER_BOUND('',#2776,.T.);
#1854=FACE_OUTER_BOUND('',#2777,.T.);
#1855=FACE_OUTER_BOUND('',#2778,.T.);
#1856=FACE_OUTER_BOUND('',#2779,.T.);
#1857=FACE_OUTER_BOUND('',#2780,.T.);
#1858=FACE_OUTER_BOUND('',#2781,.T.);
#1859=FACE_OUTER_BOUND('',#2782,.T.);
#1860=FACE_OUTER_BOUND('',#2783,.T.);
#1861=FACE_OUTER_BOUND('',#2784,.T.);
#1862=FACE_OUTER_BOUND('',#2785,.T.);
#1863=FACE_OUTER_BOUND('',#2786,.T.);
#1864=FACE_OUTER_BOUND('',#2787,.T.);
#1865=FACE_OUTER_BOUND('',#2788,.T.);
#1866=FACE_OUTER_BOUND('',#2789,.T.);
#1867=FACE_OUTER_BOUND('',#2790,.T.);
#1868=FACE_OUTER_BOUND('',#2791,.T.);
#1869=FACE_OUTER_BOUND('',#2792,.T.);
#1870=FACE_OUTER_BOUND('',#2793,.T.);
#1871=FACE_OUTER_BOUND('',#2794,.T.);
#1872=FACE_OUTER_BOUND('',#2795,.T.);
#1873=FACE_OUTER_BOUND('',#2796,.T.);
#1874=FACE_OUTER_BOUND('',#2797,.T.);
#1875=FACE_OUTER_BOUND('',#2798,.T.);
#1876=FACE_OUTER_BOUND('',#2799,.T.);
#1877=FACE_OUTER_BOUND('',#2800,.T.);
#1878=FACE_OUTER_BOUND('',#2801,.T.);
#1879=FACE_OUTER_BOUND('',#2802,.T.);
#1880=FACE_OUTER_BOUND('',#2803,.T.);
#1881=FACE_OUTER_BOUND('',#2804,.T.);
#1882=FACE_OUTER_BOUND('',#2805,.T.);
#1883=FACE_OUTER_BOUND('',#2806,.T.);
#1884=FACE_OUTER_BOUND('',#2807,.T.);
#1885=FACE_OUTER_BOUND('',#2808,.T.);
#1886=FACE_OUTER_BOUND('',#2809,.T.);
#1887=FACE_OUTER_BOUND('',#2810,.T.);
#1888=FACE_OUTER_BOUND('',#2811,.T.);
#1889=FACE_OUTER_BOUND('',#2812,.T.);
#1890=FACE_OUTER_BOUND('',#2813,.T.);
#1891=FACE_OUTER_BOUND('',#2814,.T.);
#1892=FACE_OUTER_BOUND('',#2815,.T.);
#1893=FACE_OUTER_BOUND('',#2816,.T.);
#1894=FACE_OUTER_BOUND('',#2817,.T.);
#1895=FACE_OUTER_BOUND('',#2819,.T.);
#1896=FACE_OUTER_BOUND('',#2820,.T.);
#1897=FACE_OUTER_BOUND('',#2821,.T.);
#1898=FACE_OUTER_BOUND('',#2822,.T.);
#1899=FACE_OUTER_BOUND('',#2823,.T.);
#1900=FACE_OUTER_BOUND('',#2824,.T.);
#1901=FACE_OUTER_BOUND('',#2825,.T.);
#1902=FACE_OUTER_BOUND('',#2826,.T.);
#1903=FACE_OUTER_BOUND('',#2827,.T.);
#1904=FACE_OUTER_BOUND('',#2828,.T.);
#1905=FACE_OUTER_BOUND('',#2829,.T.);
#1906=FACE_OUTER_BOUND('',#2830,.T.);
#1907=FACE_OUTER_BOUND('',#2831,.T.);
#1908=FACE_OUTER_BOUND('',#2833,.T.);
#1909=FACE_OUTER_BOUND('',#2834,.T.);
#1910=FACE_OUTER_BOUND('',#2835,.T.);
#1911=FACE_OUTER_BOUND('',#2836,.T.);
#1912=FACE_OUTER_BOUND('',#2837,.T.);
#1913=FACE_OUTER_BOUND('',#2838,.T.);
#1914=FACE_OUTER_BOUND('',#2839,.T.);
#1915=FACE_OUTER_BOUND('',#2840,.T.);
#1916=FACE_OUTER_BOUND('',#2842,.T.);
#1917=FACE_OUTER_BOUND('',#2843,.T.);
#1918=FACE_OUTER_BOUND('',#2845,.T.);
#1919=FACE_OUTER_BOUND('',#2846,.T.);
#1920=FACE_OUTER_BOUND('',#2847,.T.);
#1921=FACE_OUTER_BOUND('',#2848,.T.);
#1922=FACE_OUTER_BOUND('',#2849,.T.);
#1923=FACE_OUTER_BOUND('',#2850,.T.);
#1924=FACE_OUTER_BOUND('',#2859,.T.);
#1925=FACE_OUTER_BOUND('',#2860,.T.);
#1926=FACE_OUTER_BOUND('',#2861,.T.);
#1927=FACE_OUTER_BOUND('',#2862,.T.);
#1928=FACE_OUTER_BOUND('',#2863,.T.);
#1929=FACE_OUTER_BOUND('',#2864,.T.);
#1930=FACE_OUTER_BOUND('',#2865,.T.);
#1931=FACE_OUTER_BOUND('',#2866,.T.);
#1932=FACE_OUTER_BOUND('',#2867,.T.);
#1933=FACE_OUTER_BOUND('',#2868,.T.);
#1934=FACE_OUTER_BOUND('',#2869,.T.);
#1935=FACE_OUTER_BOUND('',#2870,.T.);
#1936=FACE_OUTER_BOUND('',#2879,.T.);
#1937=FACE_OUTER_BOUND('',#2880,.T.);
#1938=FACE_OUTER_BOUND('',#2881,.T.);
#1939=FACE_OUTER_BOUND('',#2883,.T.);
#1940=FACE_OUTER_BOUND('',#2884,.T.);
#1941=FACE_OUTER_BOUND('',#2885,.T.);
#1942=FACE_OUTER_BOUND('',#2887,.T.);
#1943=FACE_OUTER_BOUND('',#2888,.T.);
#1944=FACE_OUTER_BOUND('',#2889,.T.);
#1945=FACE_OUTER_BOUND('',#2891,.T.);
#1946=FACE_OUTER_BOUND('',#2892,.T.);
#1947=FACE_OUTER_BOUND('',#2893,.T.);
#1948=FACE_OUTER_BOUND('',#2895,.T.);
#1949=FACE_OUTER_BOUND('',#2896,.T.);
#1950=FACE_OUTER_BOUND('',#2897,.T.);
#1951=FACE_OUTER_BOUND('',#2899,.T.);
#1952=FACE_OUTER_BOUND('',#2900,.T.);
#1953=FACE_OUTER_BOUND('',#2901,.T.);
#1954=FACE_OUTER_BOUND('',#2903,.T.);
#1955=FACE_OUTER_BOUND('',#2904,.T.);
#1956=FACE_OUTER_BOUND('',#2905,.T.);
#1957=FACE_OUTER_BOUND('',#2907,.T.);
#1958=FACE_OUTER_BOUND('',#2908,.T.);
#1959=FACE_OUTER_BOUND('',#2909,.T.);
#1960=FACE_OUTER_BOUND('',#2910,.T.);
#1961=FACE_OUTER_BOUND('',#2911,.T.);
#1962=FACE_OUTER_BOUND('',#2912,.T.);
#1963=FACE_OUTER_BOUND('',#2913,.T.);
#1964=FACE_OUTER_BOUND('',#2914,.T.);
#1965=FACE_OUTER_BOUND('',#2915,.T.);
#1966=FACE_OUTER_BOUND('',#2916,.T.);
#1967=FACE_OUTER_BOUND('',#2917,.T.);
#1968=FACE_OUTER_BOUND('',#2918,.T.);
#1969=FACE_OUTER_BOUND('',#2919,.T.);
#1970=FACE_OUTER_BOUND('',#2920,.T.);
#1971=FACE_OUTER_BOUND('',#2921,.T.);
#1972=FACE_OUTER_BOUND('',#2922,.T.);
#1973=FACE_OUTER_BOUND('',#2923,.T.);
#1974=FACE_OUTER_BOUND('',#2924,.T.);
#1975=FACE_OUTER_BOUND('',#2925,.T.);
#1976=FACE_OUTER_BOUND('',#2929,.T.);
#1977=FACE_OUTER_BOUND('',#2930,.T.);
#1978=FACE_OUTER_BOUND('',#2934,.T.);
#1979=FACE_OUTER_BOUND('',#2935,.T.);
#1980=FACE_OUTER_BOUND('',#2936,.T.);
#1981=FACE_OUTER_BOUND('',#2937,.T.);
#1982=FACE_OUTER_BOUND('',#2938,.T.);
#1983=FACE_OUTER_BOUND('',#2939,.T.);
#1984=FACE_OUTER_BOUND('',#2940,.T.);
#1985=FACE_OUTER_BOUND('',#2941,.T.);
#1986=FACE_OUTER_BOUND('',#2942,.T.);
#1987=FACE_OUTER_BOUND('',#2943,.T.);
#1988=FACE_OUTER_BOUND('',#2944,.T.);
#1989=FACE_OUTER_BOUND('',#2945,.T.);
#1990=FACE_OUTER_BOUND('',#2946,.T.);
#1991=FACE_OUTER_BOUND('',#2947,.T.);
#1992=FACE_OUTER_BOUND('',#2948,.T.);
#1993=FACE_OUTER_BOUND('',#2949,.T.);
#1994=FACE_OUTER_BOUND('',#2950,.T.);
#1995=FACE_OUTER_BOUND('',#2951,.T.);
#1996=FACE_OUTER_BOUND('',#2952,.T.);
#1997=FACE_OUTER_BOUND('',#2953,.T.);
#1998=FACE_OUTER_BOUND('',#2954,.T.);
#1999=FACE_OUTER_BOUND('',#2955,.T.);
#2000=FACE_OUTER_BOUND('',#2956,.T.);
#2001=FACE_OUTER_BOUND('',#2957,.T.);
#2002=FACE_OUTER_BOUND('',#2958,.T.);
#2003=FACE_OUTER_BOUND('',#2959,.T.);
#2004=FACE_OUTER_BOUND('',#2960,.T.);
#2005=FACE_OUTER_BOUND('',#2961,.T.);
#2006=FACE_OUTER_BOUND('',#2962,.T.);
#2007=FACE_OUTER_BOUND('',#2963,.T.);
#2008=FACE_OUTER_BOUND('',#2964,.T.);
#2009=FACE_OUTER_BOUND('',#2965,.T.);
#2010=FACE_OUTER_BOUND('',#2966,.T.);
#2011=FACE_OUTER_BOUND('',#2967,.T.);
#2012=FACE_OUTER_BOUND('',#2968,.T.);
#2013=FACE_OUTER_BOUND('',#2969,.T.);
#2014=FACE_OUTER_BOUND('',#2970,.T.);
#2015=FACE_OUTER_BOUND('',#2971,.T.);
#2016=FACE_OUTER_BOUND('',#2972,.T.);
#2017=FACE_OUTER_BOUND('',#2973,.T.);
#2018=FACE_OUTER_BOUND('',#2974,.T.);
#2019=FACE_OUTER_BOUND('',#2975,.T.);
#2020=FACE_OUTER_BOUND('',#2976,.T.);
#2021=FACE_OUTER_BOUND('',#2977,.T.);
#2022=FACE_OUTER_BOUND('',#2978,.T.);
#2023=FACE_OUTER_BOUND('',#2979,.T.);
#2024=FACE_OUTER_BOUND('',#2980,.T.);
#2025=FACE_OUTER_BOUND('',#2981,.T.);
#2026=FACE_OUTER_BOUND('',#2982,.T.);
#2027=FACE_OUTER_BOUND('',#2983,.T.);
#2028=FACE_OUTER_BOUND('',#2984,.T.);
#2029=FACE_OUTER_BOUND('',#2985,.T.);
#2030=FACE_OUTER_BOUND('',#2986,.T.);
#2031=FACE_OUTER_BOUND('',#2987,.T.);
#2032=FACE_OUTER_BOUND('',#2988,.T.);
#2033=FACE_OUTER_BOUND('',#2989,.T.);
#2034=FACE_OUTER_BOUND('',#2990,.T.);
#2035=FACE_OUTER_BOUND('',#2991,.T.);
#2036=FACE_OUTER_BOUND('',#2992,.T.);
#2037=FACE_OUTER_BOUND('',#2993,.T.);
#2038=FACE_OUTER_BOUND('',#2994,.T.);
#2039=FACE_OUTER_BOUND('',#2995,.T.);
#2040=FACE_OUTER_BOUND('',#2996,.T.);
#2041=FACE_OUTER_BOUND('',#2997,.T.);
#2042=FACE_OUTER_BOUND('',#2998,.T.);
#2043=FACE_OUTER_BOUND('',#2999,.T.);
#2044=FACE_OUTER_BOUND('',#3000,.T.);
#2045=FACE_OUTER_BOUND('',#3001,.T.);
#2046=FACE_OUTER_BOUND('',#3002,.T.);
#2047=FACE_OUTER_BOUND('',#3003,.T.);
#2048=FACE_OUTER_BOUND('',#3004,.T.);
#2049=FACE_OUTER_BOUND('',#3005,.T.);
#2050=FACE_OUTER_BOUND('',#3006,.T.);
#2051=FACE_OUTER_BOUND('',#3007,.T.);
#2052=FACE_OUTER_BOUND('',#3008,.T.);
#2053=FACE_OUTER_BOUND('',#3009,.T.);
#2054=FACE_OUTER_BOUND('',#3010,.T.);
#2055=FACE_OUTER_BOUND('',#3011,.T.);
#2056=FACE_OUTER_BOUND('',#3012,.T.);
#2057=FACE_OUTER_BOUND('',#3013,.T.);
#2058=FACE_OUTER_BOUND('',#3014,.T.);
#2059=FACE_OUTER_BOUND('',#3015,.T.);
#2060=FACE_OUTER_BOUND('',#3016,.T.);
#2061=FACE_OUTER_BOUND('',#3017,.T.);
#2062=FACE_OUTER_BOUND('',#3018,.T.);
#2063=FACE_OUTER_BOUND('',#3019,.T.);
#2064=FACE_OUTER_BOUND('',#3020,.T.);
#2065=FACE_OUTER_BOUND('',#3021,.T.);
#2066=FACE_OUTER_BOUND('',#3022,.T.);
#2067=FACE_OUTER_BOUND('',#3023,.T.);
#2068=FACE_OUTER_BOUND('',#3024,.T.);
#2069=FACE_OUTER_BOUND('',#3025,.T.);
#2070=FACE_OUTER_BOUND('',#3026,.T.);
#2071=FACE_OUTER_BOUND('',#3027,.T.);
#2072=FACE_OUTER_BOUND('',#3028,.T.);
#2073=FACE_OUTER_BOUND('',#3029,.T.);
#2074=FACE_OUTER_BOUND('',#3030,.T.);
#2075=FACE_OUTER_BOUND('',#3031,.T.);
#2076=FACE_OUTER_BOUND('',#3032,.T.);
#2077=FACE_OUTER_BOUND('',#3033,.T.);
#2078=FACE_OUTER_BOUND('',#3034,.T.);
#2079=FACE_OUTER_BOUND('',#3035,.T.);
#2080=FACE_OUTER_BOUND('',#3036,.T.);
#2081=FACE_OUTER_BOUND('',#3037,.T.);
#2082=FACE_OUTER_BOUND('',#3038,.T.);
#2083=FACE_OUTER_BOUND('',#3039,.T.);
#2084=FACE_OUTER_BOUND('',#3040,.T.);
#2085=FACE_OUTER_BOUND('',#3041,.T.);
#2086=FACE_OUTER_BOUND('',#3043,.T.);
#2087=FACE_OUTER_BOUND('',#3044,.T.);
#2088=FACE_OUTER_BOUND('',#3045,.T.);
#2089=FACE_OUTER_BOUND('',#3046,.T.);
#2090=FACE_OUTER_BOUND('',#3047,.T.);
#2091=FACE_OUTER_BOUND('',#3048,.T.);
#2092=FACE_OUTER_BOUND('',#3049,.T.);
#2093=FACE_OUTER_BOUND('',#3050,.T.);
#2094=FACE_OUTER_BOUND('',#3051,.T.);
#2095=FACE_OUTER_BOUND('',#3052,.T.);
#2096=FACE_OUTER_BOUND('',#3053,.T.);
#2097=FACE_OUTER_BOUND('',#3054,.T.);
#2098=FACE_OUTER_BOUND('',#3055,.T.);
#2099=FACE_OUTER_BOUND('',#3056,.T.);
#2100=FACE_OUTER_BOUND('',#3057,.T.);
#2101=FACE_OUTER_BOUND('',#3058,.T.);
#2102=FACE_OUTER_BOUND('',#3059,.T.);
#2103=FACE_OUTER_BOUND('',#3060,.T.);
#2104=FACE_OUTER_BOUND('',#3061,.T.);
#2105=FACE_OUTER_BOUND('',#3062,.T.);
#2106=FACE_OUTER_BOUND('',#3064,.T.);
#2107=FACE_OUTER_BOUND('',#3065,.T.);
#2108=FACE_OUTER_BOUND('',#3067,.T.);
#2109=FACE_OUTER_BOUND('',#3068,.T.);
#2110=FACE_OUTER_BOUND('',#3070,.T.);
#2111=FACE_OUTER_BOUND('',#3072,.T.);
#2112=FACE_OUTER_BOUND('',#3073,.T.);
#2113=FACE_OUTER_BOUND('',#3074,.T.);
#2114=FACE_OUTER_BOUND('',#3075,.T.);
#2115=FACE_OUTER_BOUND('',#3076,.T.);
#2116=FACE_OUTER_BOUND('',#3077,.T.);
#2117=FACE_OUTER_BOUND('',#3078,.T.);
#2118=FACE_OUTER_BOUND('',#3079,.T.);
#2119=FACE_OUTER_BOUND('',#3080,.T.);
#2120=FACE_OUTER_BOUND('',#3081,.T.);
#2121=FACE_OUTER_BOUND('',#3082,.T.);
#2122=FACE_OUTER_BOUND('',#3083,.T.);
#2123=FACE_OUTER_BOUND('',#3084,.T.);
#2124=FACE_OUTER_BOUND('',#3085,.T.);
#2125=FACE_OUTER_BOUND('',#3086,.T.);
#2126=FACE_OUTER_BOUND('',#3087,.T.);
#2127=FACE_OUTER_BOUND('',#3088,.T.);
#2128=FACE_OUTER_BOUND('',#3089,.T.);
#2129=FACE_OUTER_BOUND('',#3090,.T.);
#2130=FACE_OUTER_BOUND('',#3091,.T.);
#2131=FACE_OUTER_BOUND('',#3092,.T.);
#2132=FACE_OUTER_BOUND('',#3093,.T.);
#2133=FACE_OUTER_BOUND('',#3095,.T.);
#2134=FACE_OUTER_BOUND('',#3096,.T.);
#2135=FACE_OUTER_BOUND('',#3098,.T.);
#2136=FACE_OUTER_BOUND('',#3099,.T.);
#2137=FACE_OUTER_BOUND('',#3100,.T.);
#2138=FACE_OUTER_BOUND('',#3101,.T.);
#2139=FACE_OUTER_BOUND('',#3103,.T.);
#2140=FACE_OUTER_BOUND('',#3104,.T.);
#2141=FACE_OUTER_BOUND('',#3106,.T.);
#2142=FACE_OUTER_BOUND('',#3107,.T.);
#2143=FACE_OUTER_BOUND('',#3109,.T.);
#2144=FACE_OUTER_BOUND('',#3110,.T.);
#2145=FACE_OUTER_BOUND('',#3111,.T.);
#2146=FACE_OUTER_BOUND('',#3112,.T.);
#2147=FACE_OUTER_BOUND('',#3114,.T.);
#2148=FACE_OUTER_BOUND('',#3115,.T.);
#2149=FACE_OUTER_BOUND('',#3117,.T.);
#2150=FACE_OUTER_BOUND('',#3119,.T.);
#2151=FACE_OUTER_BOUND('',#3120,.T.);
#2152=FACE_OUTER_BOUND('',#3121,.T.);
#2153=FACE_OUTER_BOUND('',#3123,.T.);
#2154=FACE_OUTER_BOUND('',#3124,.T.);
#2155=FACE_OUTER_BOUND('',#3126,.T.);
#2156=FACE_OUTER_BOUND('',#3127,.T.);
#2157=FACE_OUTER_BOUND('',#3129,.T.);
#2158=FACE_OUTER_BOUND('',#3130,.T.);
#2159=FACE_OUTER_BOUND('',#3132,.T.);
#2160=FACE_OUTER_BOUND('',#3133,.T.);
#2161=FACE_OUTER_BOUND('',#3135,.T.);
#2162=FACE_OUTER_BOUND('',#3136,.T.);
#2163=FACE_OUTER_BOUND('',#3137,.T.);
#2164=FACE_OUTER_BOUND('',#3139,.T.);
#2165=FACE_OUTER_BOUND('',#3140,.T.);
#2166=FACE_OUTER_BOUND('',#3141,.T.);
#2167=FACE_OUTER_BOUND('',#3143,.T.);
#2168=FACE_OUTER_BOUND('',#3144,.T.);
#2169=FACE_OUTER_BOUND('',#3146,.T.);
#2170=FACE_OUTER_BOUND('',#3147,.T.);
#2171=FACE_OUTER_BOUND('',#3148,.T.);
#2172=FACE_OUTER_BOUND('',#3149,.T.);
#2173=FACE_OUTER_BOUND('',#3151,.T.);
#2174=FACE_OUTER_BOUND('',#3152,.T.);
#2175=FACE_OUTER_BOUND('',#3154,.T.);
#2176=FACE_OUTER_BOUND('',#3155,.T.);
#2177=FACE_OUTER_BOUND('',#3157,.T.);
#2178=FACE_OUTER_BOUND('',#3158,.T.);
#2179=FACE_OUTER_BOUND('',#3159,.T.);
#2180=FACE_OUTER_BOUND('',#3160,.T.);
#2181=FACE_OUTER_BOUND('',#3161,.T.);
#2182=FACE_OUTER_BOUND('',#3162,.T.);
#2183=FACE_OUTER_BOUND('',#3164,.T.);
#2184=FACE_OUTER_BOUND('',#3165,.T.);
#2185=FACE_OUTER_BOUND('',#3166,.T.);
#2186=FACE_OUTER_BOUND('',#3168,.T.);
#2187=FACE_OUTER_BOUND('',#3169,.T.);
#2188=FACE_OUTER_BOUND('',#3171,.T.);
#2189=FACE_OUTER_BOUND('',#3173,.T.);
#2190=FACE_OUTER_BOUND('',#3174,.T.);
#2191=FACE_OUTER_BOUND('',#3176,.T.);
#2192=FACE_OUTER_BOUND('',#3177,.T.);
#2193=FACE_OUTER_BOUND('',#3179,.T.);
#2194=FACE_OUTER_BOUND('',#3180,.T.);
#2195=FACE_OUTER_BOUND('',#3181,.T.);
#2196=FACE_OUTER_BOUND('',#3182,.T.);
#2197=FACE_OUTER_BOUND('',#3183,.T.);
#2198=FACE_OUTER_BOUND('',#3184,.T.);
#2199=FACE_OUTER_BOUND('',#3185,.T.);
#2200=FACE_OUTER_BOUND('',#3186,.T.);
#2201=FACE_OUTER_BOUND('',#3187,.T.);
#2202=FACE_OUTER_BOUND('',#3188,.T.);
#2203=FACE_OUTER_BOUND('',#3189,.T.);
#2204=FACE_OUTER_BOUND('',#3190,.T.);
#2205=FACE_OUTER_BOUND('',#3191,.T.);
#2206=FACE_OUTER_BOUND('',#3192,.T.);
#2207=FACE_OUTER_BOUND('',#3193,.T.);
#2208=FACE_OUTER_BOUND('',#3195,.T.);
#2209=FACE_OUTER_BOUND('',#3196,.T.);
#2210=FACE_OUTER_BOUND('',#3197,.T.);
#2211=FACE_OUTER_BOUND('',#3198,.T.);
#2212=FACE_OUTER_BOUND('',#3199,.T.);
#2213=FACE_OUTER_BOUND('',#3200,.T.);
#2214=FACE_OUTER_BOUND('',#3201,.T.);
#2215=FACE_OUTER_BOUND('',#3202,.T.);
#2216=FACE_OUTER_BOUND('',#3203,.T.);
#2217=FACE_OUTER_BOUND('',#3204,.T.);
#2218=FACE_OUTER_BOUND('',#3205,.T.);
#2219=FACE_OUTER_BOUND('',#3206,.T.);
#2220=FACE_OUTER_BOUND('',#3207,.T.);
#2221=FACE_OUTER_BOUND('',#3208,.T.);
#2222=FACE_OUTER_BOUND('',#3209,.T.);
#2223=FACE_OUTER_BOUND('',#3210,.T.);
#2224=FACE_OUTER_BOUND('',#3211,.T.);
#2225=FACE_OUTER_BOUND('',#3212,.T.);
#2226=FACE_OUTER_BOUND('',#3213,.T.);
#2227=FACE_OUTER_BOUND('',#3214,.T.);
#2228=FACE_OUTER_BOUND('',#3215,.T.);
#2229=FACE_OUTER_BOUND('',#3216,.T.);
#2230=FACE_OUTER_BOUND('',#3217,.T.);
#2231=FACE_OUTER_BOUND('',#3218,.T.);
#2232=FACE_OUTER_BOUND('',#3219,.T.);
#2233=FACE_OUTER_BOUND('',#3220,.T.);
#2234=FACE_OUTER_BOUND('',#3221,.T.);
#2235=FACE_OUTER_BOUND('',#3222,.T.);
#2236=FACE_OUTER_BOUND('',#3223,.T.);
#2237=FACE_OUTER_BOUND('',#3224,.T.);
#2238=FACE_OUTER_BOUND('',#3225,.T.);
#2239=FACE_OUTER_BOUND('',#3226,.T.);
#2240=FACE_OUTER_BOUND('',#3227,.T.);
#2241=FACE_OUTER_BOUND('',#3228,.T.);
#2242=FACE_OUTER_BOUND('',#3229,.T.);
#2243=FACE_OUTER_BOUND('',#3230,.T.);
#2244=FACE_OUTER_BOUND('',#3231,.T.);
#2245=FACE_OUTER_BOUND('',#3232,.T.);
#2246=FACE_OUTER_BOUND('',#3233,.T.);
#2247=FACE_OUTER_BOUND('',#3234,.T.);
#2248=FACE_OUTER_BOUND('',#3235,.T.);
#2249=FACE_OUTER_BOUND('',#3236,.T.);
#2250=FACE_OUTER_BOUND('',#3237,.T.);
#2251=FACE_OUTER_BOUND('',#3238,.T.);
#2252=FACE_OUTER_BOUND('',#3239,.T.);
#2253=FACE_OUTER_BOUND('',#3240,.T.);
#2254=FACE_OUTER_BOUND('',#3241,.T.);
#2255=FACE_OUTER_BOUND('',#3242,.T.);
#2256=FACE_OUTER_BOUND('',#3243,.T.);
#2257=FACE_OUTER_BOUND('',#3244,.T.);
#2258=FACE_OUTER_BOUND('',#3245,.T.);
#2259=FACE_OUTER_BOUND('',#3246,.T.);
#2260=FACE_OUTER_BOUND('',#3247,.T.);
#2261=FACE_OUTER_BOUND('',#3248,.T.);
#2262=FACE_OUTER_BOUND('',#3249,.T.);
#2263=FACE_OUTER_BOUND('',#3250,.T.);
#2264=FACE_OUTER_BOUND('',#3251,.T.);
#2265=FACE_OUTER_BOUND('',#3252,.T.);
#2266=FACE_OUTER_BOUND('',#3253,.T.);
#2267=FACE_OUTER_BOUND('',#3254,.T.);
#2268=FACE_OUTER_BOUND('',#3255,.T.);
#2269=FACE_OUTER_BOUND('',#3256,.T.);
#2270=FACE_OUTER_BOUND('',#3257,.T.);
#2271=FACE_OUTER_BOUND('',#3258,.T.);
#2272=FACE_OUTER_BOUND('',#3259,.T.);
#2273=FACE_OUTER_BOUND('',#3260,.T.);
#2274=FACE_OUTER_BOUND('',#3261,.T.);
#2275=FACE_OUTER_BOUND('',#3262,.T.);
#2276=FACE_OUTER_BOUND('',#3263,.T.);
#2277=FACE_OUTER_BOUND('',#3264,.T.);
#2278=FACE_OUTER_BOUND('',#3265,.T.);
#2279=FACE_OUTER_BOUND('',#3266,.T.);
#2280=FACE_OUTER_BOUND('',#3267,.T.);
#2281=FACE_OUTER_BOUND('',#3268,.T.);
#2282=FACE_OUTER_BOUND('',#3269,.T.);
#2283=FACE_OUTER_BOUND('',#3270,.T.);
#2284=FACE_OUTER_BOUND('',#3271,.T.);
#2285=FACE_OUTER_BOUND('',#3272,.T.);
#2286=FACE_OUTER_BOUND('',#3273,.T.);
#2287=FACE_OUTER_BOUND('',#3274,.T.);
#2288=FACE_OUTER_BOUND('',#3275,.T.);
#2289=FACE_OUTER_BOUND('',#3276,.T.);
#2290=FACE_OUTER_BOUND('',#3277,.T.);
#2291=FACE_OUTER_BOUND('',#3278,.T.);
#2292=FACE_OUTER_BOUND('',#3279,.T.);
#2293=FACE_OUTER_BOUND('',#3280,.T.);
#2294=FACE_OUTER_BOUND('',#3281,.T.);
#2295=FACE_OUTER_BOUND('',#3282,.T.);
#2296=FACE_OUTER_BOUND('',#3283,.T.);
#2297=FACE_OUTER_BOUND('',#3284,.T.);
#2298=FACE_OUTER_BOUND('',#3285,.T.);
#2299=FACE_OUTER_BOUND('',#3286,.T.);
#2300=FACE_OUTER_BOUND('',#3287,.T.);
#2301=FACE_OUTER_BOUND('',#3288,.T.);
#2302=FACE_OUTER_BOUND('',#3289,.T.);
#2303=FACE_OUTER_BOUND('',#3290,.T.);
#2304=FACE_OUTER_BOUND('',#3291,.T.);
#2305=FACE_OUTER_BOUND('',#3292,.T.);
#2306=FACE_OUTER_BOUND('',#3293,.T.);
#2307=FACE_OUTER_BOUND('',#3294,.T.);
#2308=FACE_OUTER_BOUND('',#3295,.T.);
#2309=FACE_OUTER_BOUND('',#3296,.T.);
#2310=FACE_OUTER_BOUND('',#3297,.T.);
#2311=FACE_OUTER_BOUND('',#3298,.T.);
#2312=FACE_OUTER_BOUND('',#3299,.T.);
#2313=FACE_OUTER_BOUND('',#3300,.T.);
#2314=FACE_OUTER_BOUND('',#3301,.T.);
#2315=FACE_OUTER_BOUND('',#3302,.T.);
#2316=FACE_OUTER_BOUND('',#3303,.T.);
#2317=FACE_OUTER_BOUND('',#3304,.T.);
#2318=FACE_OUTER_BOUND('',#3305,.T.);
#2319=FACE_OUTER_BOUND('',#3306,.T.);
#2320=FACE_OUTER_BOUND('',#3307,.T.);
#2321=FACE_OUTER_BOUND('',#3308,.T.);
#2322=FACE_OUTER_BOUND('',#3309,.T.);
#2323=FACE_OUTER_BOUND('',#3310,.T.);
#2324=FACE_OUTER_BOUND('',#3311,.T.);
#2325=FACE_OUTER_BOUND('',#3312,.T.);
#2326=FACE_OUTER_BOUND('',#3313,.T.);
#2327=FACE_OUTER_BOUND('',#3314,.T.);
#2328=FACE_OUTER_BOUND('',#3315,.T.);
#2329=FACE_OUTER_BOUND('',#3316,.T.);
#2330=FACE_OUTER_BOUND('',#3317,.T.);
#2331=FACE_OUTER_BOUND('',#3318,.T.);
#2332=FACE_OUTER_BOUND('',#3319,.T.);
#2333=FACE_OUTER_BOUND('',#3320,.T.);
#2334=FACE_OUTER_BOUND('',#3321,.T.);
#2335=FACE_OUTER_BOUND('',#3322,.T.);
#2336=FACE_OUTER_BOUND('',#3323,.T.);
#2337=FACE_OUTER_BOUND('',#3324,.T.);
#2338=FACE_OUTER_BOUND('',#3325,.T.);
#2339=FACE_OUTER_BOUND('',#3326,.T.);
#2340=FACE_OUTER_BOUND('',#3327,.T.);
#2341=FACE_OUTER_BOUND('',#3328,.T.);
#2342=FACE_OUTER_BOUND('',#3329,.T.);
#2343=FACE_OUTER_BOUND('',#3330,.T.);
#2344=FACE_OUTER_BOUND('',#3331,.T.);
#2345=FACE_OUTER_BOUND('',#3332,.T.);
#2346=FACE_OUTER_BOUND('',#3333,.T.);
#2347=FACE_OUTER_BOUND('',#3334,.T.);
#2348=FACE_OUTER_BOUND('',#3335,.T.);
#2349=FACE_OUTER_BOUND('',#3336,.T.);
#2350=FACE_OUTER_BOUND('',#3337,.T.);
#2351=FACE_OUTER_BOUND('',#3338,.T.);
#2352=FACE_OUTER_BOUND('',#3339,.T.);
#2353=FACE_OUTER_BOUND('',#3340,.T.);
#2354=FACE_OUTER_BOUND('',#3341,.T.);
#2355=FACE_OUTER_BOUND('',#3342,.T.);
#2356=FACE_OUTER_BOUND('',#3343,.T.);
#2357=FACE_OUTER_BOUND('',#3344,.T.);
#2358=FACE_OUTER_BOUND('',#3345,.T.);
#2359=FACE_OUTER_BOUND('',#3346,.T.);
#2360=FACE_OUTER_BOUND('',#3347,.T.);
#2361=FACE_OUTER_BOUND('',#3348,.T.);
#2362=FACE_OUTER_BOUND('',#3349,.T.);
#2363=FACE_OUTER_BOUND('',#3350,.T.);
#2364=FACE_OUTER_BOUND('',#3351,.T.);
#2365=FACE_OUTER_BOUND('',#3352,.T.);
#2366=FACE_OUTER_BOUND('',#3353,.T.);
#2367=FACE_OUTER_BOUND('',#3354,.T.);
#2368=FACE_OUTER_BOUND('',#3355,.T.);
#2369=FACE_OUTER_BOUND('',#3356,.T.);
#2370=FACE_OUTER_BOUND('',#3357,.T.);
#2371=FACE_OUTER_BOUND('',#3358,.T.);
#2372=FACE_OUTER_BOUND('',#3359,.T.);
#2373=FACE_OUTER_BOUND('',#3360,.T.);
#2374=FACE_OUTER_BOUND('',#3361,.T.);
#2375=FACE_OUTER_BOUND('',#3362,.T.);
#2376=FACE_OUTER_BOUND('',#3363,.T.);
#2377=FACE_OUTER_BOUND('',#3364,.T.);
#2378=FACE_OUTER_BOUND('',#3365,.T.);
#2379=FACE_OUTER_BOUND('',#3366,.T.);
#2380=FACE_OUTER_BOUND('',#3367,.T.);
#2381=FACE_OUTER_BOUND('',#3368,.T.);
#2382=FACE_OUTER_BOUND('',#3369,.T.);
#2383=FACE_OUTER_BOUND('',#3370,.T.);
#2384=FACE_OUTER_BOUND('',#3371,.T.);
#2385=FACE_OUTER_BOUND('',#3372,.T.);
#2386=FACE_OUTER_BOUND('',#3373,.T.);
#2387=FACE_OUTER_BOUND('',#3374,.T.);
#2388=FACE_OUTER_BOUND('',#3375,.T.);
#2389=FACE_OUTER_BOUND('',#3376,.T.);
#2390=FACE_OUTER_BOUND('',#3377,.T.);
#2391=FACE_OUTER_BOUND('',#3378,.T.);
#2392=FACE_OUTER_BOUND('',#3379,.T.);
#2393=FACE_OUTER_BOUND('',#3380,.T.);
#2394=FACE_OUTER_BOUND('',#3381,.T.);
#2395=FACE_OUTER_BOUND('',#3382,.T.);
#2396=FACE_OUTER_BOUND('',#3383,.T.);
#2397=FACE_OUTER_BOUND('',#3384,.T.);
#2398=FACE_OUTER_BOUND('',#3385,.T.);
#2399=FACE_OUTER_BOUND('',#3386,.T.);
#2400=FACE_OUTER_BOUND('',#3387,.T.);
#2401=FACE_OUTER_BOUND('',#3388,.T.);
#2402=FACE_OUTER_BOUND('',#3389,.T.);
#2403=FACE_OUTER_BOUND('',#3390,.T.);
#2404=FACE_OUTER_BOUND('',#3391,.T.);
#2405=FACE_OUTER_BOUND('',#3392,.T.);
#2406=FACE_OUTER_BOUND('',#3393,.T.);
#2407=FACE_OUTER_BOUND('',#3394,.T.);
#2408=FACE_OUTER_BOUND('',#3395,.T.);
#2409=FACE_OUTER_BOUND('',#3396,.T.);
#2410=FACE_OUTER_BOUND('',#3397,.T.);
#2411=FACE_OUTER_BOUND('',#3398,.T.);
#2412=FACE_OUTER_BOUND('',#3399,.T.);
#2413=FACE_OUTER_BOUND('',#3400,.T.);
#2414=FACE_OUTER_BOUND('',#3401,.T.);
#2415=FACE_OUTER_BOUND('',#3402,.T.);
#2416=FACE_OUTER_BOUND('',#3403,.T.);
#2417=FACE_OUTER_BOUND('',#3404,.T.);
#2418=FACE_OUTER_BOUND('',#3405,.T.);
#2419=FACE_OUTER_BOUND('',#3406,.T.);
#2420=FACE_OUTER_BOUND('',#3407,.T.);
#2421=FACE_OUTER_BOUND('',#3408,.T.);
#2422=FACE_OUTER_BOUND('',#3409,.T.);
#2423=FACE_OUTER_BOUND('',#3410,.T.);
#2424=FACE_OUTER_BOUND('',#3411,.T.);
#2425=FACE_OUTER_BOUND('',#3412,.T.);
#2426=FACE_OUTER_BOUND('',#3413,.T.);
#2427=FACE_OUTER_BOUND('',#3414,.T.);
#2428=FACE_OUTER_BOUND('',#3415,.T.);
#2429=FACE_OUTER_BOUND('',#3416,.T.);
#2430=FACE_OUTER_BOUND('',#3417,.T.);
#2431=FACE_OUTER_BOUND('',#3418,.T.);
#2432=FACE_OUTER_BOUND('',#3419,.T.);
#2433=FACE_OUTER_BOUND('',#3420,.T.);
#2434=FACE_OUTER_BOUND('',#3421,.T.);
#2435=FACE_OUTER_BOUND('',#3422,.T.);
#2436=FACE_OUTER_BOUND('',#3423,.T.);
#2437=FACE_OUTER_BOUND('',#3425,.T.);
#2438=FACE_OUTER_BOUND('',#3461,.T.);
#2439=FACE_OUTER_BOUND('',#3462,.T.);
#2440=FACE_OUTER_BOUND('',#3464,.T.);
#2441=FACE_OUTER_BOUND('',#3465,.T.);
#2442=FACE_OUTER_BOUND('',#3466,.T.);
#2443=FACE_OUTER_BOUND('',#3467,.T.);
#2444=FACE_OUTER_BOUND('',#3468,.T.);
#2445=FACE_OUTER_BOUND('',#3469,.T.);
#2446=FACE_OUTER_BOUND('',#3470,.T.);
#2447=FACE_OUTER_BOUND('',#3471,.T.);
#2448=FACE_OUTER_BOUND('',#3472,.T.);
#2449=FACE_OUTER_BOUND('',#3473,.T.);
#2450=FACE_OUTER_BOUND('',#3474,.T.);
#2451=FACE_OUTER_BOUND('',#3475,.T.);
#2452=FACE_OUTER_BOUND('',#3476,.T.);
#2453=FACE_OUTER_BOUND('',#3477,.T.);
#2454=FACE_OUTER_BOUND('',#3478,.T.);
#2455=FACE_OUTER_BOUND('',#3479,.T.);
#2456=FACE_OUTER_BOUND('',#3480,.T.);
#2457=FACE_OUTER_BOUND('',#3481,.T.);
#2458=FACE_OUTER_BOUND('',#3482,.T.);
#2459=FACE_OUTER_BOUND('',#3483,.T.);
#2460=FACE_OUTER_BOUND('',#3484,.T.);
#2461=FACE_OUTER_BOUND('',#3485,.T.);
#2462=FACE_OUTER_BOUND('',#3486,.T.);
#2463=FACE_OUTER_BOUND('',#3487,.T.);
#2464=FACE_OUTER_BOUND('',#3488,.T.);
#2465=FACE_OUTER_BOUND('',#3489,.T.);
#2466=FACE_OUTER_BOUND('',#3490,.T.);
#2467=FACE_OUTER_BOUND('',#3491,.T.);
#2468=FACE_OUTER_BOUND('',#3492,.T.);
#2469=FACE_OUTER_BOUND('',#3493,.T.);
#2470=FACE_OUTER_BOUND('',#3494,.T.);
#2471=FACE_OUTER_BOUND('',#3495,.T.);
#2472=FACE_OUTER_BOUND('',#3496,.T.);
#2473=FACE_OUTER_BOUND('',#3497,.T.);
#2474=FACE_OUTER_BOUND('',#3498,.T.);
#2475=FACE_OUTER_BOUND('',#3499,.T.);
#2476=FACE_OUTER_BOUND('',#3501,.T.);
#2477=FACE_OUTER_BOUND('',#3502,.T.);
#2478=FACE_OUTER_BOUND('',#3503,.T.);
#2479=FACE_OUTER_BOUND('',#3504,.T.);
#2480=FACE_OUTER_BOUND('',#3505,.T.);
#2481=FACE_OUTER_BOUND('',#3506,.T.);
#2482=FACE_OUTER_BOUND('',#3507,.T.);
#2483=FACE_OUTER_BOUND('',#3508,.T.);
#2484=FACE_OUTER_BOUND('',#3509,.T.);
#2485=FACE_OUTER_BOUND('',#3510,.T.);
#2486=FACE_OUTER_BOUND('',#3511,.T.);
#2487=FACE_OUTER_BOUND('',#3512,.T.);
#2488=FACE_OUTER_BOUND('',#3513,.T.);
#2489=FACE_OUTER_BOUND('',#3514,.T.);
#2490=FACE_OUTER_BOUND('',#3516,.T.);
#2491=FACE_OUTER_BOUND('',#3517,.T.);
#2492=FACE_OUTER_BOUND('',#3518,.T.);
#2493=FACE_OUTER_BOUND('',#3519,.T.);
#2494=FACE_OUTER_BOUND('',#3520,.T.);
#2495=FACE_OUTER_BOUND('',#3521,.T.);
#2496=FACE_OUTER_BOUND('',#3522,.T.);
#2497=FACE_OUTER_BOUND('',#3523,.T.);
#2498=FACE_OUTER_BOUND('',#3525,.T.);
#2499=FACE_OUTER_BOUND('',#3527,.T.);
#2500=FACE_OUTER_BOUND('',#3528,.T.);
#2501=FACE_OUTER_BOUND('',#3529,.T.);
#2502=FACE_OUTER_BOUND('',#3530,.T.);
#2503=FACE_OUTER_BOUND('',#3531,.T.);
#2504=EDGE_LOOP('',(#9799,#9800,#9801,#9802));
#2505=EDGE_LOOP('',(#9803,#9804,#9805,#9806,#9807,#9808));
#2506=EDGE_LOOP('',(#9809));
#2507=EDGE_LOOP('',(#9810));
#2508=EDGE_LOOP('',(#9811,#9812,#9813,#9814));
#2509=EDGE_LOOP('',(#9815,#9816,#9817,#9818,#9819,#9820));
#2510=EDGE_LOOP('',(#9821));
#2511=EDGE_LOOP('',(#9822,#9823,#9824,#9825));
#2512=EDGE_LOOP('',(#9826,#9827,#9828,#9829));
#2513=EDGE_LOOP('',(#9830));
#2514=EDGE_LOOP('',(#9831));
#2515=EDGE_LOOP('',(#9832,#9833,#9834,#9835,#9836,#9837));
#2516=EDGE_LOOP('',(#9838,#9839,#9840,#9841));
#2517=EDGE_LOOP('',(#9842,#9843,#9844,#9845,#9846,#9847));
#2518=EDGE_LOOP('',(#9848));
#2519=EDGE_LOOP('',(#9849,#9850,#9851,#9852));
#2520=EDGE_LOOP('',(#9853,#9854,#9855,#9856));
#2521=EDGE_LOOP('',(#9857,#9858,#9859,#9860,#9861,#9862));
#2522=EDGE_LOOP('',(#9863,#9864,#9865,#9866));
#2523=EDGE_LOOP('',(#9867,#9868,#9869,#9870,#9871,#9872,#9873,#9874));
#2524=EDGE_LOOP('',(#9875));
#2525=EDGE_LOOP('',(#9876));
#2526=EDGE_LOOP('',(#9877));
#2527=EDGE_LOOP('',(#9878));
#2528=EDGE_LOOP('',(#9879));
#2529=EDGE_LOOP('',(#9880,#9881,#9882,#9883));
#2530=EDGE_LOOP('',(#9884,#9885,#9886,#9887));
#2531=EDGE_LOOP('',(#9888,#9889,#9890,#9891));
#2532=EDGE_LOOP('',(#9892,#9893,#9894,#9895));
#2533=EDGE_LOOP('',(#9896,#9897,#9898,#9899));
#2534=EDGE_LOOP('',(#9900,#9901,#9902,#9903));
#2535=EDGE_LOOP('',(#9904,#9905,#9906,#9907));
#2536=EDGE_LOOP('',(#9908,#9909,#9910,#9911,#9912));
#2537=EDGE_LOOP('',(#9913,#9914,#9915,#9916));
#2538=EDGE_LOOP('',(#9917,#9918,#9919,#9920,#9921,#9922,#9923,#9924,#9925,
#9926));
#2539=EDGE_LOOP('',(#9927,#9928,#9929,#9930));
#2540=EDGE_LOOP('',(#9931,#9932,#9933,#9934,#9935,#9936,#9937,#9938,#9939,
#9940,#9941,#9942,#9943));
#2541=EDGE_LOOP('',(#9944,#9945,#9946,#9947));
#2542=EDGE_LOOP('',(#9948,#9949,#9950,#9951,#9952));
#2543=EDGE_LOOP('',(#9953,#9954,#9955,#9956));
#2544=EDGE_LOOP('',(#9957,#9958,#9959,#9960,#9961,#9962,#9963,#9964,#9965,
#9966,#9967,#9968,#9969,#9970,#9971,#9972,#9973,#9974));
#2545=EDGE_LOOP('',(#9975,#9976,#9977,#9978,#9979));
#2546=EDGE_LOOP('',(#9980,#9981,#9982,#9983));
#2547=EDGE_LOOP('',(#9984,#9985,#9986,#9987,#9988,#9989,#9990,#9991,#9992,
#9993));
#2548=EDGE_LOOP('',(#9994,#9995,#9996,#9997));
#2549=EDGE_LOOP('',(#9998,#9999,#10000,#10001,#10002,#10003,#10004,#10005,
#10006,#10007,#10008,#10009,#10010));
#2550=EDGE_LOOP('',(#10011,#10012,#10013,#10014));
#2551=EDGE_LOOP('',(#10015,#10016,#10017,#10018,#10019));
#2552=EDGE_LOOP('',(#10020,#10021,#10022,#10023));
#2553=EDGE_LOOP('',(#10024,#10025,#10026,#10027,#10028,#10029,#10030,#10031,
#10032,#10033,#10034,#10035,#10036,#10037,#10038,#10039,#10040,#10041));
#2554=EDGE_LOOP('',(#10042,#10043,#10044,#10045));
#2555=EDGE_LOOP('',(#10046,#10047,#10048,#10049,#10050,#10051,#10052,#10053));
#2556=EDGE_LOOP('',(#10054));
#2557=EDGE_LOOP('',(#10055));
#2558=EDGE_LOOP('',(#10056));
#2559=EDGE_LOOP('',(#10057,#10058,#10059,#10060));
#2560=EDGE_LOOP('',(#10061,#10062,#10063,#10064));
#2561=EDGE_LOOP('',(#10065,#10066,#10067,#10068));
#2562=EDGE_LOOP('',(#10069,#10070,#10071,#10072));
#2563=EDGE_LOOP('',(#10073,#10074,#10075,#10076));
#2564=EDGE_LOOP('',(#10077,#10078,#10079,#10080));
#2565=EDGE_LOOP('',(#10081,#10082,#10083,#10084));
#2566=EDGE_LOOP('',(#10085,#10086,#10087,#10088));
#2567=EDGE_LOOP('',(#10089,#10090,#10091,#10092));
#2568=EDGE_LOOP('',(#10093,#10094,#10095,#10096));
#2569=EDGE_LOOP('',(#10097,#10098,#10099,#10100));
#2570=EDGE_LOOP('',(#10101,#10102,#10103,#10104,#10105,#10106));
#2571=EDGE_LOOP('',(#10107,#10108,#10109,#10110,#10111));
#2572=EDGE_LOOP('',(#10112,#10113,#10114,#10115));
#2573=EDGE_LOOP('',(#10116,#10117,#10118,#10119,#10120));
#2574=EDGE_LOOP('',(#10121,#10122,#10123,#10124));
#2575=EDGE_LOOP('',(#10125,#10126,#10127,#10128));
#2576=EDGE_LOOP('',(#10129,#10130,#10131,#10132));
#2577=EDGE_LOOP('',(#10133,#10134,#10135,#10136,#10137,#10138));
#2578=EDGE_LOOP('',(#10139,#10140,#10141,#10142,#10143));
#2579=EDGE_LOOP('',(#10144,#10145,#10146,#10147));
#2580=EDGE_LOOP('',(#10148,#10149,#10150,#10151,#10152));
#2581=EDGE_LOOP('',(#10153,#10154,#10155,#10156));
#2582=EDGE_LOOP('',(#10157,#10158,#10159,#10160));
#2583=EDGE_LOOP('',(#10161,#10162,#10163,#10164));
#2584=EDGE_LOOP('',(#10165,#10166,#10167,#10168,#10169));
#2585=EDGE_LOOP('',(#10170,#10171,#10172,#10173));
#2586=EDGE_LOOP('',(#10174,#10175,#10176,#10177,#10178));
#2587=EDGE_LOOP('',(#10179,#10180,#10181,#10182));
#2588=EDGE_LOOP('',(#10183,#10184,#10185,#10186));
#2589=EDGE_LOOP('',(#10187,#10188,#10189,#10190,#10191));
#2590=EDGE_LOOP('',(#10192,#10193,#10194,#10195,#10196));
#2591=EDGE_LOOP('',(#10197,#10198,#10199,#10200));
#2592=EDGE_LOOP('',(#10201,#10202,#10203,#10204,#10205));
#2593=EDGE_LOOP('',(#10206,#10207,#10208,#10209));
#2594=EDGE_LOOP('',(#10210,#10211,#10212,#10213,#10214));
#2595=EDGE_LOOP('',(#10215,#10216,#10217,#10218));
#2596=EDGE_LOOP('',(#10219,#10220,#10221,#10222,#10223));
#2597=EDGE_LOOP('',(#10224,#10225,#10226,#10227));
#2598=EDGE_LOOP('',(#10228,#10229,#10230,#10231,#10232));
#2599=EDGE_LOOP('',(#10233,#10234,#10235,#10236));
#2600=EDGE_LOOP('',(#10237,#10238,#10239,#10240));
#2601=EDGE_LOOP('',(#10241,#10242,#10243,#10244));
#2602=EDGE_LOOP('',(#10245,#10246,#10247,#10248));
#2603=EDGE_LOOP('',(#10249,#10250,#10251,#10252));
#2604=EDGE_LOOP('',(#10253,#10254,#10255,#10256));
#2605=EDGE_LOOP('',(#10257,#10258,#10259,#10260));
#2606=EDGE_LOOP('',(#10261,#10262,#10263,#10264));
#2607=EDGE_LOOP('',(#10265,#10266,#10267,#10268));
#2608=EDGE_LOOP('',(#10269,#10270,#10271,#10272,#10273,#10274));
#2609=EDGE_LOOP('',(#10275,#10276,#10277,#10278,#10279,#10280));
#2610=EDGE_LOOP('',(#10281,#10282,#10283,#10284,#10285));
#2611=EDGE_LOOP('',(#10286,#10287,#10288,#10289,#10290));
#2612=EDGE_LOOP('',(#10291,#10292,#10293,#10294));
#2613=EDGE_LOOP('',(#10295,#10296,#10297,#10298));
#2614=EDGE_LOOP('',(#10299,#10300,#10301));
#2615=EDGE_LOOP('',(#10302,#10303,#10304,#10305));
#2616=EDGE_LOOP('',(#10306,#10307,#10308));
#2617=EDGE_LOOP('',(#10309,#10310,#10311,#10312,#10313));
#2618=EDGE_LOOP('',(#10314,#10315,#10316));
#2619=EDGE_LOOP('',(#10317,#10318,#10319,#10320));
#2620=EDGE_LOOP('',(#10321,#10322,#10323));
#2621=EDGE_LOOP('',(#10324,#10325,#10326,#10327,#10328));
#2622=EDGE_LOOP('',(#10329,#10330,#10331,#10332,#10333,#10334));
#2623=EDGE_LOOP('',(#10335));
#2624=EDGE_LOOP('',(#10336));
#2625=EDGE_LOOP('',(#10337));
#2626=EDGE_LOOP('',(#10338));
#2627=EDGE_LOOP('',(#10339,#10340,#10341,#10342));
#2628=EDGE_LOOP('',(#10343));
#2629=EDGE_LOOP('',(#10344));
#2630=EDGE_LOOP('',(#10345,#10346,#10347,#10348));
#2631=EDGE_LOOP('',(#10349));
#2632=EDGE_LOOP('',(#10350));
#2633=EDGE_LOOP('',(#10351,#10352,#10353,#10354));
#2634=EDGE_LOOP('',(#10355));
#2635=EDGE_LOOP('',(#10356));
#2636=EDGE_LOOP('',(#10357));
#2637=EDGE_LOOP('',(#10358));
#2638=EDGE_LOOP('',(#10359,#10360,#10361,#10362));
#2639=EDGE_LOOP('',(#10363,#10364,#10365,#10366));
#2640=EDGE_LOOP('',(#10367,#10368));
#2641=EDGE_LOOP('',(#10369,#10370));
#2642=EDGE_LOOP('',(#10371,#10372,#10373,#10374,#10375));
#2643=EDGE_LOOP('',(#10376));
#2644=EDGE_LOOP('',(#10377));
#2645=EDGE_LOOP('',(#10378,#10379,#10380,#10381,#10382));
#2646=EDGE_LOOP('',(#10383,#10384,#10385,#10386));
#2647=EDGE_LOOP('',(#10387,#10388,#10389,#10390,#10391,#10392,#10393,#10394));
#2648=EDGE_LOOP('',(#10395));
#2649=EDGE_LOOP('',(#10396,#10397,#10398,#10399,#10400,#10401,#10402));
#2650=EDGE_LOOP('',(#10403,#10404,#10405,#10406,#10407));
#2651=EDGE_LOOP('',(#10408,#10409,#10410,#10411));
#2652=EDGE_LOOP('',(#10412,#10413,#10414,#10415));
#2653=EDGE_LOOP('',(#10416,#10417,#10418,#10419));
#2654=EDGE_LOOP('',(#10420,#10421,#10422,#10423));
#2655=EDGE_LOOP('',(#10424,#10425,#10426,#10427));
#2656=EDGE_LOOP('',(#10428,#10429,#10430,#10431));
#2657=EDGE_LOOP('',(#10432,#10433,#10434,#10435));
#2658=EDGE_LOOP('',(#10436,#10437,#10438));
#2659=EDGE_LOOP('',(#10439,#10440,#10441,#10442,#10443,#10444,#10445,#10446,
#10447,#10448,#10449,#10450));
#2660=EDGE_LOOP('',(#10451,#10452,#10453,#10454,#10455,#10456,#10457,#10458,
#10459,#10460,#10461,#10462));
#2661=EDGE_LOOP('',(#10463,#10464,#10465,#10466));
#2662=EDGE_LOOP('',(#10467,#10468,#10469,#10470,#10471));
#2663=EDGE_LOOP('',(#10472,#10473,#10474,#10475));
#2664=EDGE_LOOP('',(#10476,#10477,#10478,#10479));
#2665=EDGE_LOOP('',(#10480,#10481,#10482,#10483));
#2666=EDGE_LOOP('',(#10484,#10485,#10486,#10487));
#2667=EDGE_LOOP('',(#10488,#10489,#10490,#10491));
#2668=EDGE_LOOP('',(#10492,#10493,#10494,#10495));
#2669=EDGE_LOOP('',(#10496,#10497,#10498));
#2670=EDGE_LOOP('',(#10499,#10500,#10501,#10502,#10503,#10504,#10505,#10506,
#10507,#10508,#10509,#10510));
#2671=EDGE_LOOP('',(#10511,#10512,#10513,#10514,#10515,#10516,#10517,#10518,
#10519,#10520,#10521,#10522));
#2672=EDGE_LOOP('',(#10523,#10524,#10525,#10526));
#2673=EDGE_LOOP('',(#10527,#10528,#10529,#10530));
#2674=EDGE_LOOP('',(#10531,#10532,#10533,#10534));
#2675=EDGE_LOOP('',(#10535,#10536,#10537,#10538,#10539));
#2676=EDGE_LOOP('',(#10540,#10541,#10542,#10543));
#2677=EDGE_LOOP('',(#10544,#10545,#10546,#10547));
#2678=EDGE_LOOP('',(#10548,#10549,#10550,#10551));
#2679=EDGE_LOOP('',(#10552,#10553,#10554,#10555));
#2680=EDGE_LOOP('',(#10556,#10557,#10558,#10559,#10560,#10561,#10562,#10563,
#10564,#10565,#10566,#10567));
#2681=EDGE_LOOP('',(#10568,#10569,#10570,#10571));
#2682=EDGE_LOOP('',(#10572,#10573,#10574,#10575));
#2683=EDGE_LOOP('',(#10576,#10577,#10578,#10579));
#2684=EDGE_LOOP('',(#10580,#10581,#10582,#10583));
#2685=EDGE_LOOP('',(#10584,#10585,#10586,#10587));
#2686=EDGE_LOOP('',(#10588,#10589,#10590,#10591,#10592));
#2687=EDGE_LOOP('',(#10593,#10594,#10595,#10596));
#2688=EDGE_LOOP('',(#10597,#10598,#10599,#10600));
#2689=EDGE_LOOP('',(#10601,#10602,#10603));
#2690=EDGE_LOOP('',(#10604,#10605,#10606,#10607,#10608,#10609,#10610,#10611,
#10612,#10613,#10614,#10615));
#2691=EDGE_LOOP('',(#10616,#10617,#10618,#10619,#10620,#10621,#10622,#10623,
#10624,#10625,#10626,#10627));
#2692=EDGE_LOOP('',(#10628,#10629,#10630,#10631));
#2693=EDGE_LOOP('',(#10632,#10633,#10634,#10635));
#2694=EDGE_LOOP('',(#10636,#10637,#10638,#10639,#10640));
#2695=EDGE_LOOP('',(#10641,#10642,#10643,#10644));
#2696=EDGE_LOOP('',(#10645,#10646,#10647,#10648));
#2697=EDGE_LOOP('',(#10649,#10650,#10651,#10652));
#2698=EDGE_LOOP('',(#10653,#10654,#10655,#10656,#10657,#10658,#10659,#10660,
#10661,#10662,#10663));
#2699=EDGE_LOOP('',(#10664,#10665,#10666,#10667,#10668));
#2700=EDGE_LOOP('',(#10669,#10670,#10671,#10672));
#2701=EDGE_LOOP('',(#10673,#10674,#10675,#10676));
#2702=EDGE_LOOP('',(#10677,#10678,#10679,#10680));
#2703=EDGE_LOOP('',(#10681,#10682,#10683,#10684));
#2704=EDGE_LOOP('',(#10685,#10686,#10687,#10688));
#2705=EDGE_LOOP('',(#10689,#10690,#10691,#10692,#10693,#10694,#10695,#10696));
#2706=EDGE_LOOP('',(#10697,#10698,#10699,#10700,#10701,#10702,#10703,#10704,
#10705,#10706,#10707,#10708,#10709,#10710,#10711,#10712,#10713,#10714,#10715,
#10716));
#2707=EDGE_LOOP('',(#10717,#10718,#10719,#10720));
#2708=EDGE_LOOP('',(#10721,#10722,#10723,#10724));
#2709=EDGE_LOOP('',(#10725));
#2710=EDGE_LOOP('',(#10726));
#2711=EDGE_LOOP('',(#10727));
#2712=EDGE_LOOP('',(#10728));
#2713=EDGE_LOOP('',(#10729));
#2714=EDGE_LOOP('',(#10730,#10731,#10732,#10733));
#2715=EDGE_LOOP('',(#10734,#10735,#10736,#10737));
#2716=EDGE_LOOP('',(#10738,#10739,#10740,#10741));
#2717=EDGE_LOOP('',(#10742,#10743,#10744,#10745));
#2718=EDGE_LOOP('',(#10746,#10747,#10748,#10749));
#2719=EDGE_LOOP('',(#10750,#10751,#10752,#10753));
#2720=EDGE_LOOP('',(#10754,#10755,#10756,#10757));
#2721=EDGE_LOOP('',(#10758,#10759,#10760,#10761));
#2722=EDGE_LOOP('',(#10762,#10763,#10764,#10765,#10766,#10767,#10768));
#2723=EDGE_LOOP('',(#10769,#10770,#10771,#10772,#10773,#10774));
#2724=EDGE_LOOP('',(#10775,#10776,#10777,#10778));
#2725=EDGE_LOOP('',(#10779,#10780,#10781,#10782));
#2726=EDGE_LOOP('',(#10783,#10784,#10785));
#2727=EDGE_LOOP('',(#10786,#10787,#10788,#10789));
#2728=EDGE_LOOP('',(#10790,#10791,#10792,#10793));
#2729=EDGE_LOOP('',(#10794,#10795,#10796,#10797));
#2730=EDGE_LOOP('',(#10798,#10799,#10800));
#2731=EDGE_LOOP('',(#10801,#10802,#10803,#10804));
#2732=EDGE_LOOP('',(#10805,#10806,#10807));
#2733=EDGE_LOOP('',(#10808,#10809,#10810,#10811));
#2734=EDGE_LOOP('',(#10812,#10813,#10814,#10815));
#2735=EDGE_LOOP('',(#10816,#10817,#10818,#10819));
#2736=EDGE_LOOP('',(#10820,#10821,#10822));
#2737=EDGE_LOOP('',(#10823,#10824,#10825));
#2738=EDGE_LOOP('',(#10826,#10827,#10828,#10829));
#2739=EDGE_LOOP('',(#10830,#10831,#10832,#10833,#10834,#10835,#10836,#10837,
#10838,#10839,#10840,#10841));
#2740=EDGE_LOOP('',(#10842,#10843,#10844));
#2741=EDGE_LOOP('',(#10845,#10846,#10847));
#2742=EDGE_LOOP('',(#10848,#10849,#10850,#10851));
#2743=EDGE_LOOP('',(#10852,#10853,#10854,#10855,#10856));
#2744=EDGE_LOOP('',(#10857,#10858,#10859,#10860,#10861));
#2745=EDGE_LOOP('',(#10862,#10863,#10864));
#2746=EDGE_LOOP('',(#10865,#10866,#10867,#10868,#10869,#10870,#10871,#10872,
#10873,#10874,#10875,#10876));
#2747=EDGE_LOOP('',(#10877));
#2748=EDGE_LOOP('',(#10878));
#2749=EDGE_LOOP('',(#10879));
#2750=EDGE_LOOP('',(#10880));
#2751=EDGE_LOOP('',(#10881));
#2752=EDGE_LOOP('',(#10882,#10883,#10884,#10885,#10886));
#2753=EDGE_LOOP('',(#10887,#10888,#10889,#10890,#10891));
#2754=EDGE_LOOP('',(#10892,#10893,#10894,#10895));
#2755=EDGE_LOOP('',(#10896,#10897,#10898,#10899));
#2756=EDGE_LOOP('',(#10900,#10901,#10902,#10903));
#2757=EDGE_LOOP('',(#10904,#10905,#10906,#10907,#10908));
#2758=EDGE_LOOP('',(#10909,#10910,#10911,#10912));
#2759=EDGE_LOOP('',(#10913));
#2760=EDGE_LOOP('',(#10914));
#2761=EDGE_LOOP('',(#10915));
#2762=EDGE_LOOP('',(#10916,#10917));
#2763=EDGE_LOOP('',(#10918,#10919,#10920,#10921));
#2764=EDGE_LOOP('',(#10922,#10923,#10924,#10925));
#2765=EDGE_LOOP('',(#10926));
#2766=EDGE_LOOP('',(#10927,#10928,#10929,#10930));
#2767=EDGE_LOOP('',(#10931,#10932,#10933,#10934,#10935,#10936));
#2768=EDGE_LOOP('',(#10937,#10938,#10939,#10940));
#2769=EDGE_LOOP('',(#10941,#10942,#10943,#10944));
#2770=EDGE_LOOP('',(#10945));
#2771=EDGE_LOOP('',(#10946,#10947,#10948,#10949));
#2772=EDGE_LOOP('',(#10950,#10951,#10952,#10953));
#2773=EDGE_LOOP('',(#10954));
#2774=EDGE_LOOP('',(#10955,#10956,#10957,#10958));
#2775=EDGE_LOOP('',(#10959,#10960,#10961,#10962));
#2776=EDGE_LOOP('',(#10963,#10964,#10965,#10966));
#2777=EDGE_LOOP('',(#10967,#10968,#10969,#10970,#10971,#10972,#10973,#10974));
#2778=EDGE_LOOP('',(#10975,#10976,#10977,#10978));
#2779=EDGE_LOOP('',(#10979,#10980,#10981,#10982));
#2780=EDGE_LOOP('',(#10983,#10984,#10985,#10986));
#2781=EDGE_LOOP('',(#10987,#10988,#10989,#10990));
#2782=EDGE_LOOP('',(#10991,#10992,#10993));
#2783=EDGE_LOOP('',(#10994,#10995,#10996));
#2784=EDGE_LOOP('',(#10997,#10998,#10999,#11000));
#2785=EDGE_LOOP('',(#11001,#11002,#11003,#11004,#11005));
#2786=EDGE_LOOP('',(#11006,#11007,#11008,#11009,#11010,#11011,#11012,#11013));
#2787=EDGE_LOOP('',(#11014,#11015,#11016,#11017));
#2788=EDGE_LOOP('',(#11018,#11019,#11020,#11021,#11022,#11023));
#2789=EDGE_LOOP('',(#11024,#11025,#11026,#11027,#11028));
#2790=EDGE_LOOP('',(#11029,#11030,#11031,#11032,#11033));
#2791=EDGE_LOOP('',(#11034,#11035,#11036,#11037));
#2792=EDGE_LOOP('',(#11038,#11039,#11040));
#2793=EDGE_LOOP('',(#11041,#11042,#11043,#11044,#11045,#11046,#11047,#11048));
#2794=EDGE_LOOP('',(#11049,#11050,#11051,#11052,#11053));
#2795=EDGE_LOOP('',(#11054,#11055,#11056,#11057,#11058,#11059,#11060,#11061,
#11062,#11063,#11064));
#2796=EDGE_LOOP('',(#11065,#11066,#11067,#11068));
#2797=EDGE_LOOP('',(#11069,#11070,#11071));
#2798=EDGE_LOOP('',(#11072,#11073,#11074));
#2799=EDGE_LOOP('',(#11075,#11076,#11077));
#2800=EDGE_LOOP('',(#11078,#11079,#11080,#11081));
#2801=EDGE_LOOP('',(#11082,#11083,#11084,#11085));
#2802=EDGE_LOOP('',(#11086,#11087,#11088,#11089));
#2803=EDGE_LOOP('',(#11090,#11091,#11092,#11093,#11094));
#2804=EDGE_LOOP('',(#11095,#11096,#11097,#11098));
#2805=EDGE_LOOP('',(#11099,#11100,#11101,#11102,#11103));
#2806=EDGE_LOOP('',(#11104,#11105,#11106,#11107));
#2807=EDGE_LOOP('',(#11108,#11109,#11110,#11111,#11112));
#2808=EDGE_LOOP('',(#11113,#11114,#11115,#11116));
#2809=EDGE_LOOP('',(#11117,#11118,#11119));
#2810=EDGE_LOOP('',(#11120,#11121,#11122,#11123));
#2811=EDGE_LOOP('',(#11124,#11125,#11126,#11127,#11128));
#2812=EDGE_LOOP('',(#11129,#11130,#11131,#11132));
#2813=EDGE_LOOP('',(#11133,#11134,#11135,#11136));
#2814=EDGE_LOOP('',(#11137,#11138,#11139,#11140));
#2815=EDGE_LOOP('',(#11141,#11142,#11143,#11144));
#2816=EDGE_LOOP('',(#11145,#11146,#11147,#11148));
#2817=EDGE_LOOP('',(#11149,#11150,#11151,#11152));
#2818=EDGE_LOOP('',(#11153));
#2819=EDGE_LOOP('',(#11154,#11155,#11156,#11157));
#2820=EDGE_LOOP('',(#11158));
#2821=EDGE_LOOP('',(#11159));
#2822=EDGE_LOOP('',(#11160));
#2823=EDGE_LOOP('',(#11161));
#2824=EDGE_LOOP('',(#11162));
#2825=EDGE_LOOP('',(#11163));
#2826=EDGE_LOOP('',(#11164));
#2827=EDGE_LOOP('',(#11165));
#2828=EDGE_LOOP('',(#11166));
#2829=EDGE_LOOP('',(#11167));
#2830=EDGE_LOOP('',(#11168,#11169,#11170,#11171));
#2831=EDGE_LOOP('',(#11172));
#2832=EDGE_LOOP('',(#11173));
#2833=EDGE_LOOP('',(#11174,#11175,#11176,#11177));
#2834=EDGE_LOOP('',(#11178));
#2835=EDGE_LOOP('',(#11179,#11180,#11181,#11182));
#2836=EDGE_LOOP('',(#11183,#11184,#11185,#11186));
#2837=EDGE_LOOP('',(#11187,#11188,#11189,#11190));
#2838=EDGE_LOOP('',(#11191,#11192,#11193,#11194,#11195,#11196,#11197,#11198));
#2839=EDGE_LOOP('',(#11199,#11200,#11201,#11202));
#2840=EDGE_LOOP('',(#11203,#11204,#11205,#11206));
#2841=EDGE_LOOP('',(#11207));
#2842=EDGE_LOOP('',(#11208,#11209,#11210,#11211));
#2843=EDGE_LOOP('',(#11212,#11213,#11214,#11215));
#2844=EDGE_LOOP('',(#11216));
#2845=EDGE_LOOP('',(#11217,#11218,#11219,#11220));
#2846=EDGE_LOOP('',(#11221,#11222,#11223,#11224,#11225,#11226,#11227,#11228));
#2847=EDGE_LOOP('',(#11229,#11230,#11231,#11232));
#2848=EDGE_LOOP('',(#11233,#11234,#11235,#11236));
#2849=EDGE_LOOP('',(#11237,#11238,#11239,#11240,#11241));
#2850=EDGE_LOOP('',(#11242));
#2851=EDGE_LOOP('',(#11243));
#2852=EDGE_LOOP('',(#11244));
#2853=EDGE_LOOP('',(#11245));
#2854=EDGE_LOOP('',(#11246));
#2855=EDGE_LOOP('',(#11247));
#2856=EDGE_LOOP('',(#11248));
#2857=EDGE_LOOP('',(#11249));
#2858=EDGE_LOOP('',(#11250,#11251,#11252,#11253));
#2859=EDGE_LOOP('',(#11254,#11255,#11256,#11257,#11258));
#2860=EDGE_LOOP('',(#11259,#11260,#11261,#11262));
#2861=EDGE_LOOP('',(#11263,#11264,#11265,#11266));
#2862=EDGE_LOOP('',(#11267,#11268,#11269,#11270));
#2863=EDGE_LOOP('',(#11271,#11272,#11273,#11274));
#2864=EDGE_LOOP('',(#11275,#11276,#11277,#11278));
#2865=EDGE_LOOP('',(#11279,#11280,#11281,#11282,#11283,#11284,#11285,#11286));
#2866=EDGE_LOOP('',(#11287,#11288,#11289,#11290));
#2867=EDGE_LOOP('',(#11291,#11292,#11293,#11294));
#2868=EDGE_LOOP('',(#11295,#11296,#11297,#11298));
#2869=EDGE_LOOP('',(#11299,#11300,#11301,#11302));
#2870=EDGE_LOOP('',(#11303));
#2871=EDGE_LOOP('',(#11304,#11305,#11306,#11307));
#2872=EDGE_LOOP('',(#11308));
#2873=EDGE_LOOP('',(#11309));
#2874=EDGE_LOOP('',(#11310));
#2875=EDGE_LOOP('',(#11311));
#2876=EDGE_LOOP('',(#11312));
#2877=EDGE_LOOP('',(#11313));
#2878=EDGE_LOOP('',(#11314));
#2879=EDGE_LOOP('',(#11315,#11316,#11317,#11318));
#2880=EDGE_LOOP('',(#11319,#11320,#11321,#11322));
#2881=EDGE_LOOP('',(#11323));
#2882=EDGE_LOOP('',(#11324));
#2883=EDGE_LOOP('',(#11325,#11326,#11327,#11328));
#2884=EDGE_LOOP('',(#11329,#11330,#11331,#11332));
#2885=EDGE_LOOP('',(#11333));
#2886=EDGE_LOOP('',(#11334));
#2887=EDGE_LOOP('',(#11335,#11336,#11337,#11338));
#2888=EDGE_LOOP('',(#11339,#11340,#11341,#11342));
#2889=EDGE_LOOP('',(#11343));
#2890=EDGE_LOOP('',(#11344));
#2891=EDGE_LOOP('',(#11345,#11346,#11347,#11348));
#2892=EDGE_LOOP('',(#11349,#11350,#11351,#11352));
#2893=EDGE_LOOP('',(#11353));
#2894=EDGE_LOOP('',(#11354));
#2895=EDGE_LOOP('',(#11355,#11356,#11357,#11358));
#2896=EDGE_LOOP('',(#11359,#11360,#11361,#11362));
#2897=EDGE_LOOP('',(#11363));
#2898=EDGE_LOOP('',(#11364));
#2899=EDGE_LOOP('',(#11365,#11366,#11367,#11368));
#2900=EDGE_LOOP('',(#11369,#11370,#11371,#11372));
#2901=EDGE_LOOP('',(#11373));
#2902=EDGE_LOOP('',(#11374));
#2903=EDGE_LOOP('',(#11375,#11376,#11377,#11378));
#2904=EDGE_LOOP('',(#11379,#11380,#11381,#11382));
#2905=EDGE_LOOP('',(#11383));
#2906=EDGE_LOOP('',(#11384));
#2907=EDGE_LOOP('',(#11385,#11386,#11387,#11388));
#2908=EDGE_LOOP('',(#11389,#11390,#11391,#11392));
#2909=EDGE_LOOP('',(#11393,#11394,#11395,#11396));
#2910=EDGE_LOOP('',(#11397,#11398,#11399,#11400));
#2911=EDGE_LOOP('',(#11401,#11402,#11403,#11404));
#2912=EDGE_LOOP('',(#11405,#11406,#11407,#11408));
#2913=EDGE_LOOP('',(#11409,#11410,#11411,#11412));
#2914=EDGE_LOOP('',(#11413,#11414,#11415,#11416));
#2915=EDGE_LOOP('',(#11417,#11418,#11419,#11420));
#2916=EDGE_LOOP('',(#11421,#11422,#11423,#11424));
#2917=EDGE_LOOP('',(#11425,#11426,#11427,#11428));
#2918=EDGE_LOOP('',(#11429,#11430,#11431,#11432));
#2919=EDGE_LOOP('',(#11433,#11434,#11435,#11436));
#2920=EDGE_LOOP('',(#11437,#11438,#11439,#11440,#11441,#11442,#11443,#11444));
#2921=EDGE_LOOP('',(#11445,#11446,#11447,#11448,#11449,#11450,#11451,#11452));
#2922=EDGE_LOOP('',(#11453,#11454,#11455,#11456,#11457,#11458,#11459,#11460));
#2923=EDGE_LOOP('',(#11461,#11462,#11463,#11464,#11465,#11466,#11467,#11468));
#2924=EDGE_LOOP('',(#11469,#11470,#11471,#11472));
#2925=EDGE_LOOP('',(#11473));
#2926=EDGE_LOOP('',(#11474,#11475,#11476,#11477));
#2927=EDGE_LOOP('',(#11478,#11479,#11480,#11481));
#2928=EDGE_LOOP('',(#11482));
#2929=EDGE_LOOP('',(#11483,#11484,#11485,#11486));
#2930=EDGE_LOOP('',(#11487));
#2931=EDGE_LOOP('',(#11488,#11489,#11490,#11491));
#2932=EDGE_LOOP('',(#11492,#11493,#11494,#11495));
#2933=EDGE_LOOP('',(#11496));
#2934=EDGE_LOOP('',(#11497,#11498,#11499,#11500));
#2935=EDGE_LOOP('',(#11501,#11502,#11503,#11504));
#2936=EDGE_LOOP('',(#11505,#11506,#11507,#11508,#11509,#11510));
#2937=EDGE_LOOP('',(#11511,#11512,#11513,#11514,#11515,#11516,#11517));
#2938=EDGE_LOOP('',(#11518,#11519,#11520,#11521));
#2939=EDGE_LOOP('',(#11522,#11523,#11524,#11525,#11526,#11527,#11528));
#2940=EDGE_LOOP('',(#11529,#11530,#11531,#11532));
#2941=EDGE_LOOP('',(#11533,#11534,#11535,#11536));
#2942=EDGE_LOOP('',(#11537,#11538,#11539,#11540,#11541,#11542));
#2943=EDGE_LOOP('',(#11543,#11544,#11545,#11546,#11547,#11548,#11549));
#2944=EDGE_LOOP('',(#11550,#11551,#11552,#11553));
#2945=EDGE_LOOP('',(#11554,#11555,#11556,#11557,#11558,#11559,#11560));
#2946=EDGE_LOOP('',(#11561,#11562,#11563,#11564));
#2947=EDGE_LOOP('',(#11565,#11566,#11567,#11568));
#2948=EDGE_LOOP('',(#11569,#11570,#11571,#11572,#11573,#11574));
#2949=EDGE_LOOP('',(#11575,#11576,#11577,#11578,#11579,#11580,#11581));
#2950=EDGE_LOOP('',(#11582,#11583,#11584,#11585));
#2951=EDGE_LOOP('',(#11586,#11587,#11588,#11589,#11590,#11591,#11592));
#2952=EDGE_LOOP('',(#11593,#11594,#11595,#11596));
#2953=EDGE_LOOP('',(#11597,#11598,#11599,#11600));
#2954=EDGE_LOOP('',(#11601,#11602,#11603,#11604,#11605,#11606));
#2955=EDGE_LOOP('',(#11607,#11608,#11609,#11610,#11611,#11612,#11613));
#2956=EDGE_LOOP('',(#11614,#11615,#11616,#11617));
#2957=EDGE_LOOP('',(#11618,#11619,#11620,#11621,#11622,#11623,#11624));
#2958=EDGE_LOOP('',(#11625,#11626,#11627,#11628));
#2959=EDGE_LOOP('',(#11629,#11630,#11631,#11632,#11633,#11634,#11635));
#2960=EDGE_LOOP('',(#11636,#11637,#11638,#11639));
#2961=EDGE_LOOP('',(#11640,#11641,#11642,#11643,#11644,#11645));
#2962=EDGE_LOOP('',(#11646,#11647,#11648,#11649,#11650,#11651,#11652));
#2963=EDGE_LOOP('',(#11653,#11654,#11655,#11656,#11657,#11658));
#2964=EDGE_LOOP('',(#11659,#11660,#11661,#11662,#11663,#11664,#11665,#11666,
#11667,#11668,#11669,#11670,#11671,#11672,#11673,#11674,#11675,#11676,#11677,
#11678,#11679,#11680,#11681,#11682,#11683,#11684,#11685,#11686,#11687,#11688,
#11689,#11690,#11691,#11692,#11693,#11694,#11695,#11696,#11697,#11698,#11699,
#11700,#11701,#11702,#11703,#11704,#11705,#11706,#11707,#11708,#11709,#11710,
#11711,#11712,#11713,#11714));
#2965=EDGE_LOOP('',(#11715,#11716,#11717,#11718));
#2966=EDGE_LOOP('',(#11719,#11720,#11721,#11722));
#2967=EDGE_LOOP('',(#11723,#11724,#11725,#11726,#11727,#11728));
#2968=EDGE_LOOP('',(#11729,#11730,#11731,#11732,#11733,#11734,#11735));
#2969=EDGE_LOOP('',(#11736,#11737,#11738,#11739));
#2970=EDGE_LOOP('',(#11740,#11741,#11742,#11743,#11744,#11745,#11746));
#2971=EDGE_LOOP('',(#11747,#11748,#11749,#11750));
#2972=EDGE_LOOP('',(#11751,#11752,#11753,#11754));
#2973=EDGE_LOOP('',(#11755,#11756,#11757,#11758,#11759,#11760));
#2974=EDGE_LOOP('',(#11761,#11762,#11763,#11764,#11765,#11766,#11767));
#2975=EDGE_LOOP('',(#11768,#11769,#11770,#11771));
#2976=EDGE_LOOP('',(#11772,#11773,#11774,#11775,#11776,#11777,#11778));
#2977=EDGE_LOOP('',(#11779,#11780,#11781,#11782));
#2978=EDGE_LOOP('',(#11783,#11784,#11785,#11786));
#2979=EDGE_LOOP('',(#11787,#11788,#11789,#11790));
#2980=EDGE_LOOP('',(#11791,#11792,#11793,#11794));
#2981=EDGE_LOOP('',(#11795,#11796,#11797,#11798));
#2982=EDGE_LOOP('',(#11799,#11800,#11801,#11802));
#2983=EDGE_LOOP('',(#11803,#11804,#11805,#11806));
#2984=EDGE_LOOP('',(#11807,#11808,#11809,#11810));
#2985=EDGE_LOOP('',(#11811,#11812,#11813,#11814));
#2986=EDGE_LOOP('',(#11815,#11816,#11817,#11818));
#2987=EDGE_LOOP('',(#11819,#11820,#11821,#11822));
#2988=EDGE_LOOP('',(#11823,#11824,#11825,#11826));
#2989=EDGE_LOOP('',(#11827,#11828,#11829,#11830));
#2990=EDGE_LOOP('',(#11831,#11832,#11833,#11834));
#2991=EDGE_LOOP('',(#11835,#11836,#11837,#11838));
#2992=EDGE_LOOP('',(#11839,#11840,#11841,#11842));
#2993=EDGE_LOOP('',(#11843,#11844,#11845,#11846));
#2994=EDGE_LOOP('',(#11847,#11848,#11849,#11850));
#2995=EDGE_LOOP('',(#11851,#11852,#11853,#11854));
#2996=EDGE_LOOP('',(#11855,#11856,#11857,#11858));
#2997=EDGE_LOOP('',(#11859,#11860,#11861,#11862));
#2998=EDGE_LOOP('',(#11863,#11864,#11865,#11866));
#2999=EDGE_LOOP('',(#11867,#11868,#11869,#11870));
#3000=EDGE_LOOP('',(#11871,#11872,#11873,#11874));
#3001=EDGE_LOOP('',(#11875,#11876,#11877,#11878));
#3002=EDGE_LOOP('',(#11879,#11880,#11881,#11882));
#3003=EDGE_LOOP('',(#11883,#11884,#11885,#11886,#11887,#11888));
#3004=EDGE_LOOP('',(#11889,#11890,#11891,#11892,#11893,#11894,#11895));
#3005=EDGE_LOOP('',(#11896,#11897,#11898,#11899));
#3006=EDGE_LOOP('',(#11900,#11901,#11902,#11903,#11904,#11905,#11906));
#3007=EDGE_LOOP('',(#11907,#11908,#11909,#11910));
#3008=EDGE_LOOP('',(#11911,#11912,#11913,#11914));
#3009=EDGE_LOOP('',(#11915,#11916,#11917,#11918,#11919,#11920,#11921));
#3010=EDGE_LOOP('',(#11922,#11923,#11924,#11925,#11926,#11927,#11928));
#3011=EDGE_LOOP('',(#11929,#11930,#11931,#11932));
#3012=EDGE_LOOP('',(#11933,#11934,#11935,#11936,#11937,#11938,#11939));
#3013=EDGE_LOOP('',(#11940,#11941,#11942,#11943));
#3014=EDGE_LOOP('',(#11944,#11945,#11946,#11947));
#3015=EDGE_LOOP('',(#11948,#11949,#11950,#11951,#11952,#11953));
#3016=EDGE_LOOP('',(#11954,#11955,#11956,#11957,#11958,#11959,#11960));
#3017=EDGE_LOOP('',(#11961,#11962,#11963,#11964));
#3018=EDGE_LOOP('',(#11965,#11966,#11967,#11968,#11969,#11970,#11971));
#3019=EDGE_LOOP('',(#11972,#11973,#11974,#11975));
#3020=EDGE_LOOP('',(#11976,#11977,#11978,#11979));
#3021=EDGE_LOOP('',(#11980,#11981,#11982,#11983,#11984,#11985));
#3022=EDGE_LOOP('',(#11986,#11987,#11988,#11989,#11990,#11991,#11992));
#3023=EDGE_LOOP('',(#11993,#11994,#11995,#11996));
#3024=EDGE_LOOP('',(#11997,#11998,#11999,#12000,#12001,#12002,#12003));
#3025=EDGE_LOOP('',(#12004,#12005,#12006,#12007));
#3026=EDGE_LOOP('',(#12008,#12009,#12010,#12011));
#3027=EDGE_LOOP('',(#12012,#12013,#12014,#12015,#12016,#12017));
#3028=EDGE_LOOP('',(#12018,#12019,#12020,#12021));
#3029=EDGE_LOOP('',(#12022,#12023,#12024,#12025,#12026,#12027,#12028));
#3030=EDGE_LOOP('',(#12029,#12030,#12031,#12032,#12033,#12034));
#3031=EDGE_LOOP('',(#12035,#12036,#12037,#12038));
#3032=EDGE_LOOP('',(#12039,#12040,#12041,#12042));
#3033=EDGE_LOOP('',(#12043,#12044,#12045,#12046));
#3034=EDGE_LOOP('',(#12047,#12048,#12049,#12050));
#3035=EDGE_LOOP('',(#12051,#12052,#12053,#12054,#12055,#12056));
#3036=EDGE_LOOP('',(#12057,#12058,#12059,#12060));
#3037=EDGE_LOOP('',(#12061,#12062,#12063,#12064,#12065,#12066,#12067));
#3038=EDGE_LOOP('',(#12068,#12069,#12070,#12071,#12072,#12073));
#3039=EDGE_LOOP('',(#12074,#12075,#12076,#12077));
#3040=EDGE_LOOP('',(#12078,#12079,#12080,#12081));
#3041=EDGE_LOOP('',(#12082,#12083,#12084,#12085,#12086,#12087,#12088,#12089,
#12090,#12091,#12092,#12093,#12094,#12095,#12096,#12097,#12098,#12099,#12100,
#12101,#12102,#12103,#12104,#12105,#12106,#12107,#12108,#12109,#12110,#12111,
#12112,#12113,#12114,#12115,#12116,#12117,#12118,#12119,#12120,#12121,#12122,
#12123,#12124,#12125,#12126,#12127,#12128,#12129,#12130,#12131,#12132,#12133));
#3042=EDGE_LOOP('',(#12134));
#3043=EDGE_LOOP('',(#12135));
#3044=EDGE_LOOP('',(#12136,#12137,#12138,#12139));
#3045=EDGE_LOOP('',(#12140,#12141,#12142,#12143));
#3046=EDGE_LOOP('',(#12144,#12145,#12146,#12147));
#3047=EDGE_LOOP('',(#12148,#12149,#12150,#12151));
#3048=EDGE_LOOP('',(#12152,#12153,#12154,#12155));
#3049=EDGE_LOOP('',(#12156,#12157,#12158,#12159,#12160,#12161,#12162));
#3050=EDGE_LOOP('',(#12163,#12164,#12165,#12166,#12167,#12168));
#3051=EDGE_LOOP('',(#12169,#12170,#12171,#12172,#12173,#12174));
#3052=EDGE_LOOP('',(#12175,#12176,#12177,#12178,#12179,#12180));
#3053=EDGE_LOOP('',(#12181,#12182,#12183,#12184,#12185,#12186));
#3054=EDGE_LOOP('',(#12187,#12188,#12189,#12190));
#3055=EDGE_LOOP('',(#12191,#12192,#12193,#12194,#12195,#12196));
#3056=EDGE_LOOP('',(#12197,#12198,#12199,#12200,#12201,#12202));
#3057=EDGE_LOOP('',(#12203,#12204,#12205,#12206,#12207,#12208));
#3058=EDGE_LOOP('',(#12209,#12210,#12211,#12212,#12213,#12214));
#3059=EDGE_LOOP('',(#12215,#12216,#12217,#12218,#12219,#12220));
#3060=EDGE_LOOP('',(#12221,#12222,#12223,#12224,#12225,#12226,#12227));
#3061=EDGE_LOOP('',(#12228,#12229,#12230,#12231,#12232,#12233));
#3062=EDGE_LOOP('',(#12234));
#3063=EDGE_LOOP('',(#12235));
#3064=EDGE_LOOP('',(#12236,#12237,#12238,#12239));
#3065=EDGE_LOOP('',(#12240));
#3066=EDGE_LOOP('',(#12241));
#3067=EDGE_LOOP('',(#12242,#12243,#12244,#12245));
#3068=EDGE_LOOP('',(#12246));
#3069=EDGE_LOOP('',(#12247));
#3070=EDGE_LOOP('',(#12248,#12249,#12250,#12251));
#3071=EDGE_LOOP('',(#12252,#12253,#12254,#12255));
#3072=EDGE_LOOP('',(#12256,#12257,#12258,#12259));
#3073=EDGE_LOOP('',(#12260));
#3074=EDGE_LOOP('',(#12261,#12262,#12263,#12264,#12265,#12266));
#3075=EDGE_LOOP('',(#12267,#12268,#12269,#12270));
#3076=EDGE_LOOP('',(#12271,#12272,#12273,#12274,#12275,#12276));
#3077=EDGE_LOOP('',(#12277,#12278,#12279,#12280,#12281,#12282));
#3078=EDGE_LOOP('',(#12283,#12284,#12285,#12286,#12287,#12288));
#3079=EDGE_LOOP('',(#12289,#12290,#12291,#12292));
#3080=EDGE_LOOP('',(#12293,#12294,#12295,#12296,#12297,#12298));
#3081=EDGE_LOOP('',(#12299,#12300,#12301,#12302,#12303,#12304));
#3082=EDGE_LOOP('',(#12305,#12306,#12307,#12308));
#3083=EDGE_LOOP('',(#12309,#12310,#12311,#12312,#12313,#12314));
#3084=EDGE_LOOP('',(#12315,#12316,#12317,#12318,#12319,#12320));
#3085=EDGE_LOOP('',(#12321,#12322,#12323,#12324));
#3086=EDGE_LOOP('',(#12325,#12326,#12327,#12328,#12329,#12330));
#3087=EDGE_LOOP('',(#12331,#12332,#12333,#12334,#12335,#12336));
#3088=EDGE_LOOP('',(#12337,#12338,#12339,#12340,#12341,#12342));
#3089=EDGE_LOOP('',(#12343,#12344,#12345,#12346));
#3090=EDGE_LOOP('',(#12347,#12348,#12349,#12350,#12351,#12352));
#3091=EDGE_LOOP('',(#12353,#12354,#12355,#12356));
#3092=EDGE_LOOP('',(#12357,#12358,#12359,#12360));
#3093=EDGE_LOOP('',(#12361));
#3094=EDGE_LOOP('',(#12362));
#3095=EDGE_LOOP('',(#12363,#12364,#12365,#12366));
#3096=EDGE_LOOP('',(#12367));
#3097=EDGE_LOOP('',(#12368));
#3098=EDGE_LOOP('',(#12369,#12370,#12371,#12372));
#3099=EDGE_LOOP('',(#12373,#12374,#12375,#12376));
#3100=EDGE_LOOP('',(#12377,#12378,#12379,#12380));
#3101=EDGE_LOOP('',(#12381));
#3102=EDGE_LOOP('',(#12382));
#3103=EDGE_LOOP('',(#12383,#12384,#12385,#12386));
#3104=EDGE_LOOP('',(#12387));
#3105=EDGE_LOOP('',(#12388));
#3106=EDGE_LOOP('',(#12389,#12390,#12391,#12392));
#3107=EDGE_LOOP('',(#12393));
#3108=EDGE_LOOP('',(#12394));
#3109=EDGE_LOOP('',(#12395,#12396,#12397,#12398));
#3110=EDGE_LOOP('',(#12399,#12400,#12401,#12402));
#3111=EDGE_LOOP('',(#12403,#12404,#12405,#12406));
#3112=EDGE_LOOP('',(#12407));
#3113=EDGE_LOOP('',(#12408));
#3114=EDGE_LOOP('',(#12409,#12410,#12411,#12412));
#3115=EDGE_LOOP('',(#12413));
#3116=EDGE_LOOP('',(#12414));
#3117=EDGE_LOOP('',(#12415));
#3118=EDGE_LOOP('',(#12416));
#3119=EDGE_LOOP('',(#12417,#12418,#12419,#12420));
#3120=EDGE_LOOP('',(#12421,#12422,#12423,#12424));
#3121=EDGE_LOOP('',(#12425));
#3122=EDGE_LOOP('',(#12426));
#3123=EDGE_LOOP('',(#12427,#12428,#12429,#12430));
#3124=EDGE_LOOP('',(#12431));
#3125=EDGE_LOOP('',(#12432));
#3126=EDGE_LOOP('',(#12433,#12434,#12435,#12436));
#3127=EDGE_LOOP('',(#12437));
#3128=EDGE_LOOP('',(#12438));
#3129=EDGE_LOOP('',(#12439,#12440,#12441,#12442));
#3130=EDGE_LOOP('',(#12443));
#3131=EDGE_LOOP('',(#12444));
#3132=EDGE_LOOP('',(#12445,#12446,#12447,#12448,#12449));
#3133=EDGE_LOOP('',(#12450));
#3134=EDGE_LOOP('',(#12451));
#3135=EDGE_LOOP('',(#12452,#12453,#12454,#12455,#12456));
#3136=EDGE_LOOP('',(#12457,#12458,#12459,#12460,#12461));
#3137=EDGE_LOOP('',(#12462));
#3138=EDGE_LOOP('',(#12463));
#3139=EDGE_LOOP('',(#12464,#12465,#12466,#12467,#12468));
#3140=EDGE_LOOP('',(#12469,#12470,#12471,#12472));
#3141=EDGE_LOOP('',(#12473));
#3142=EDGE_LOOP('',(#12474));
#3143=EDGE_LOOP('',(#12475,#12476,#12477,#12478));
#3144=EDGE_LOOP('',(#12479));
#3145=EDGE_LOOP('',(#12480));
#3146=EDGE_LOOP('',(#12481,#12482,#12483,#12484));
#3147=EDGE_LOOP('',(#12485,#12486,#12487,#12488));
#3148=EDGE_LOOP('',(#12489,#12490,#12491,#12492));
#3149=EDGE_LOOP('',(#12493));
#3150=EDGE_LOOP('',(#12494));
#3151=EDGE_LOOP('',(#12495,#12496,#12497,#12498,#12499));
#3152=EDGE_LOOP('',(#12500));
#3153=EDGE_LOOP('',(#12501));
#3154=EDGE_LOOP('',(#12502,#12503,#12504,#12505,#12506));
#3155=EDGE_LOOP('',(#12507));
#3156=EDGE_LOOP('',(#12508));
#3157=EDGE_LOOP('',(#12509,#12510,#12511,#12512));
#3158=EDGE_LOOP('',(#12513,#12514,#12515,#12516));
#3159=EDGE_LOOP('',(#12517,#12518,#12519,#12520));
#3160=EDGE_LOOP('',(#12521,#12522,#12523,#12524,#12525,#12526));
#3161=EDGE_LOOP('',(#12527,#12528,#12529,#12530));
#3162=EDGE_LOOP('',(#12531));
#3163=EDGE_LOOP('',(#12532));
#3164=EDGE_LOOP('',(#12533,#12534,#12535,#12536));
#3165=EDGE_LOOP('',(#12537,#12538,#12539,#12540));
#3166=EDGE_LOOP('',(#12541));
#3167=EDGE_LOOP('',(#12542));
#3168=EDGE_LOOP('',(#12543,#12544,#12545,#12546));
#3169=EDGE_LOOP('',(#12547));
#3170=EDGE_LOOP('',(#12548));
#3171=EDGE_LOOP('',(#12549,#12550,#12551,#12552,#12553,#12554,#12555));
#3172=EDGE_LOOP('',(#12556));
#3173=EDGE_LOOP('',(#12557,#12558,#12559,#12560,#12561,#12562));
#3174=EDGE_LOOP('',(#12563));
#3175=EDGE_LOOP('',(#12564));
#3176=EDGE_LOOP('',(#12565,#12566,#12567,#12568,#12569));
#3177=EDGE_LOOP('',(#12570));
#3178=EDGE_LOOP('',(#12571,#12572,#12573,#12574,#12575,#12576,#12577,#12578,
#12579,#12580,#12581,#12582,#12583,#12584));
#3179=EDGE_LOOP('',(#12585,#12586,#12587,#12588,#12589));
#3180=EDGE_LOOP('',(#12590,#12591,#12592,#12593));
#3181=EDGE_LOOP('',(#12594,#12595,#12596,#12597));
#3182=EDGE_LOOP('',(#12598,#12599,#12600,#12601));
#3183=EDGE_LOOP('',(#12602,#12603,#12604,#12605));
#3184=EDGE_LOOP('',(#12606,#12607,#12608,#12609));
#3185=EDGE_LOOP('',(#12610,#12611,#12612,#12613));
#3186=EDGE_LOOP('',(#12614,#12615,#12616,#12617));
#3187=EDGE_LOOP('',(#12618,#12619,#12620,#12621));
#3188=EDGE_LOOP('',(#12622,#12623,#12624,#12625));
#3189=EDGE_LOOP('',(#12626,#12627,#12628,#12629));
#3190=EDGE_LOOP('',(#12630,#12631,#12632,#12633));
#3191=EDGE_LOOP('',(#12634,#12635,#12636,#12637));
#3192=EDGE_LOOP('',(#12638,#12639,#12640,#12641));
#3193=EDGE_LOOP('',(#12642));
#3194=EDGE_LOOP('',(#12643,#12644,#12645,#12646,#12647,#12648,#12649,#12650,
#12651,#12652,#12653,#12654,#12655,#12656));
#3195=EDGE_LOOP('',(#12657,#12658,#12659,#12660));
#3196=EDGE_LOOP('',(#12661,#12662,#12663,#12664));
#3197=EDGE_LOOP('',(#12665,#12666,#12667,#12668));
#3198=EDGE_LOOP('',(#12669,#12670,#12671,#12672));
#3199=EDGE_LOOP('',(#12673,#12674,#12675,#12676));
#3200=EDGE_LOOP('',(#12677,#12678,#12679,#12680));
#3201=EDGE_LOOP('',(#12681,#12682,#12683,#12684));
#3202=EDGE_LOOP('',(#12685,#12686,#12687,#12688));
#3203=EDGE_LOOP('',(#12689,#12690,#12691,#12692));
#3204=EDGE_LOOP('',(#12693,#12694,#12695,#12696));
#3205=EDGE_LOOP('',(#12697,#12698,#12699,#12700));
#3206=EDGE_LOOP('',(#12701,#12702,#12703,#12704));
#3207=EDGE_LOOP('',(#12705,#12706,#12707,#12708));
#3208=EDGE_LOOP('',(#12709,#12710,#12711,#12712));
#3209=EDGE_LOOP('',(#12713,#12714,#12715,#12716));
#3210=EDGE_LOOP('',(#12717,#12718,#12719,#12720));
#3211=EDGE_LOOP('',(#12721,#12722,#12723,#12724));
#3212=EDGE_LOOP('',(#12725,#12726,#12727,#12728));
#3213=EDGE_LOOP('',(#12729,#12730,#12731,#12732));
#3214=EDGE_LOOP('',(#12733,#12734,#12735,#12736));
#3215=EDGE_LOOP('',(#12737,#12738,#12739,#12740));
#3216=EDGE_LOOP('',(#12741,#12742,#12743,#12744));
#3217=EDGE_LOOP('',(#12745,#12746,#12747,#12748));
#3218=EDGE_LOOP('',(#12749,#12750,#12751,#12752));
#3219=EDGE_LOOP('',(#12753,#12754,#12755,#12756));
#3220=EDGE_LOOP('',(#12757,#12758,#12759,#12760));
#3221=EDGE_LOOP('',(#12761,#12762,#12763,#12764));
#3222=EDGE_LOOP('',(#12765,#12766,#12767,#12768));
#3223=EDGE_LOOP('',(#12769,#12770,#12771,#12772));
#3224=EDGE_LOOP('',(#12773,#12774,#12775,#12776));
#3225=EDGE_LOOP('',(#12777,#12778,#12779,#12780));
#3226=EDGE_LOOP('',(#12781,#12782,#12783,#12784));
#3227=EDGE_LOOP('',(#12785,#12786,#12787,#12788));
#3228=EDGE_LOOP('',(#12789,#12790,#12791,#12792));
#3229=EDGE_LOOP('',(#12793,#12794,#12795,#12796));
#3230=EDGE_LOOP('',(#12797,#12798,#12799,#12800));
#3231=EDGE_LOOP('',(#12801,#12802,#12803,#12804));
#3232=EDGE_LOOP('',(#12805,#12806,#12807,#12808));
#3233=EDGE_LOOP('',(#12809,#12810,#12811,#12812));
#3234=EDGE_LOOP('',(#12813,#12814,#12815,#12816));
#3235=EDGE_LOOP('',(#12817,#12818,#12819,#12820));
#3236=EDGE_LOOP('',(#12821,#12822,#12823,#12824));
#3237=EDGE_LOOP('',(#12825,#12826,#12827,#12828));
#3238=EDGE_LOOP('',(#12829,#12830,#12831,#12832));
#3239=EDGE_LOOP('',(#12833,#12834,#12835,#12836));
#3240=EDGE_LOOP('',(#12837,#12838,#12839,#12840));
#3241=EDGE_LOOP('',(#12841,#12842,#12843,#12844));
#3242=EDGE_LOOP('',(#12845,#12846,#12847,#12848));
#3243=EDGE_LOOP('',(#12849,#12850,#12851,#12852));
#3244=EDGE_LOOP('',(#12853,#12854,#12855,#12856));
#3245=EDGE_LOOP('',(#12857,#12858,#12859,#12860));
#3246=EDGE_LOOP('',(#12861,#12862,#12863,#12864));
#3247=EDGE_LOOP('',(#12865,#12866,#12867,#12868));
#3248=EDGE_LOOP('',(#12869,#12870,#12871,#12872));
#3249=EDGE_LOOP('',(#12873,#12874,#12875,#12876));
#3250=EDGE_LOOP('',(#12877,#12878,#12879,#12880));
#3251=EDGE_LOOP('',(#12881,#12882,#12883,#12884));
#3252=EDGE_LOOP('',(#12885,#12886,#12887,#12888));
#3253=EDGE_LOOP('',(#12889,#12890,#12891,#12892));
#3254=EDGE_LOOP('',(#12893,#12894,#12895,#12896));
#3255=EDGE_LOOP('',(#12897,#12898,#12899,#12900));
#3256=EDGE_LOOP('',(#12901,#12902,#12903,#12904));
#3257=EDGE_LOOP('',(#12905,#12906,#12907,#12908));
#3258=EDGE_LOOP('',(#12909,#12910,#12911,#12912));
#3259=EDGE_LOOP('',(#12913,#12914,#12915,#12916));
#3260=EDGE_LOOP('',(#12917,#12918,#12919,#12920));
#3261=EDGE_LOOP('',(#12921,#12922,#12923,#12924));
#3262=EDGE_LOOP('',(#12925,#12926,#12927,#12928));
#3263=EDGE_LOOP('',(#12929,#12930,#12931,#12932));
#3264=EDGE_LOOP('',(#12933,#12934,#12935,#12936));
#3265=EDGE_LOOP('',(#12937,#12938,#12939,#12940,#12941,#12942,#12943,#12944,
#12945,#12946,#12947,#12948,#12949,#12950,#12951,#12952,#12953,#12954,#12955,
#12956,#12957,#12958,#12959,#12960,#12961,#12962,#12963,#12964,#12965,#12966,
#12967,#12968,#12969,#12970,#12971,#12972,#12973,#12974,#12975,#12976,#12977,
#12978,#12979,#12980,#12981,#12982,#12983,#12984,#12985,#12986,#12987,#12988,
#12989,#12990,#12991,#12992,#12993,#12994,#12995,#12996,#12997,#12998,#12999,
#13000,#13001,#13002,#13003,#13004,#13005,#13006,#13007,#13008));
#3266=EDGE_LOOP('',(#13009,#13010,#13011,#13012,#13013));
#3267=EDGE_LOOP('',(#13014,#13015,#13016,#13017));
#3268=EDGE_LOOP('',(#13018,#13019,#13020,#13021,#13022,#13023,#13024,#13025,
#13026,#13027,#13028,#13029,#13030,#13031,#13032,#13033,#13034,#13035,#13036,
#13037,#13038,#13039,#13040,#13041,#13042,#13043,#13044,#13045,#13046,#13047,
#13048,#13049,#13050,#13051,#13052,#13053,#13054,#13055,#13056,#13057,#13058,
#13059,#13060,#13061,#13062,#13063,#13064,#13065,#13066,#13067,#13068,#13069,
#13070,#13071,#13072,#13073,#13074,#13075,#13076,#13077,#13078,#13079,#13080,
#13081,#13082,#13083,#13084,#13085,#13086,#13087,#13088,#13089));
#3269=EDGE_LOOP('',(#13090,#13091,#13092,#13093));
#3270=EDGE_LOOP('',(#13094,#13095,#13096));
#3271=EDGE_LOOP('',(#13097,#13098,#13099,#13100));
#3272=EDGE_LOOP('',(#13101,#13102,#13103));
#3273=EDGE_LOOP('',(#13104,#13105,#13106,#13107));
#3274=EDGE_LOOP('',(#13108,#13109,#13110));
#3275=EDGE_LOOP('',(#13111,#13112,#13113,#13114));
#3276=EDGE_LOOP('',(#13115,#13116,#13117));
#3277=EDGE_LOOP('',(#13118,#13119,#13120,#13121));
#3278=EDGE_LOOP('',(#13122,#13123,#13124));
#3279=EDGE_LOOP('',(#13125,#13126,#13127,#13128));
#3280=EDGE_LOOP('',(#13129,#13130,#13131));
#3281=EDGE_LOOP('',(#13132,#13133,#13134,#13135));
#3282=EDGE_LOOP('',(#13136,#13137,#13138));
#3283=EDGE_LOOP('',(#13139,#13140,#13141,#13142));
#3284=EDGE_LOOP('',(#13143,#13144,#13145));
#3285=EDGE_LOOP('',(#13146,#13147,#13148,#13149));
#3286=EDGE_LOOP('',(#13150,#13151,#13152));
#3287=EDGE_LOOP('',(#13153,#13154,#13155,#13156));
#3288=EDGE_LOOP('',(#13157,#13158,#13159));
#3289=EDGE_LOOP('',(#13160,#13161,#13162,#13163));
#3290=EDGE_LOOP('',(#13164,#13165,#13166));
#3291=EDGE_LOOP('',(#13167,#13168,#13169,#13170));
#3292=EDGE_LOOP('',(#13171,#13172,#13173));
#3293=EDGE_LOOP('',(#13174,#13175,#13176,#13177));
#3294=EDGE_LOOP('',(#13178,#13179,#13180));
#3295=EDGE_LOOP('',(#13181,#13182,#13183,#13184));
#3296=EDGE_LOOP('',(#13185,#13186,#13187));
#3297=EDGE_LOOP('',(#13188,#13189,#13190,#13191));
#3298=EDGE_LOOP('',(#13192,#13193,#13194));
#3299=EDGE_LOOP('',(#13195,#13196,#13197,#13198));
#3300=EDGE_LOOP('',(#13199,#13200,#13201));
#3301=EDGE_LOOP('',(#13202,#13203,#13204,#13205));
#3302=EDGE_LOOP('',(#13206,#13207,#13208));
#3303=EDGE_LOOP('',(#13209,#13210,#13211,#13212));
#3304=EDGE_LOOP('',(#13213,#13214,#13215));
#3305=EDGE_LOOP('',(#13216,#13217,#13218,#13219));
#3306=EDGE_LOOP('',(#13220,#13221,#13222));
#3307=EDGE_LOOP('',(#13223,#13224,#13225,#13226));
#3308=EDGE_LOOP('',(#13227,#13228,#13229));
#3309=EDGE_LOOP('',(#13230,#13231,#13232,#13233));
#3310=EDGE_LOOP('',(#13234,#13235,#13236));
#3311=EDGE_LOOP('',(#13237,#13238,#13239,#13240));
#3312=EDGE_LOOP('',(#13241,#13242,#13243));
#3313=EDGE_LOOP('',(#13244,#13245,#13246,#13247));
#3314=EDGE_LOOP('',(#13248,#13249,#13250));
#3315=EDGE_LOOP('',(#13251,#13252,#13253,#13254));
#3316=EDGE_LOOP('',(#13255,#13256,#13257));
#3317=EDGE_LOOP('',(#13258,#13259,#13260,#13261));
#3318=EDGE_LOOP('',(#13262,#13263,#13264));
#3319=EDGE_LOOP('',(#13265,#13266,#13267,#13268));
#3320=EDGE_LOOP('',(#13269,#13270,#13271));
#3321=EDGE_LOOP('',(#13272,#13273,#13274,#13275));
#3322=EDGE_LOOP('',(#13276,#13277,#13278));
#3323=EDGE_LOOP('',(#13279,#13280,#13281,#13282));
#3324=EDGE_LOOP('',(#13283,#13284,#13285));
#3325=EDGE_LOOP('',(#13286,#13287,#13288,#13289));
#3326=EDGE_LOOP('',(#13290,#13291,#13292));
#3327=EDGE_LOOP('',(#13293,#13294,#13295,#13296));
#3328=EDGE_LOOP('',(#13297,#13298,#13299));
#3329=EDGE_LOOP('',(#13300,#13301,#13302,#13303));
#3330=EDGE_LOOP('',(#13304,#13305,#13306));
#3331=EDGE_LOOP('',(#13307,#13308,#13309,#13310));
#3332=EDGE_LOOP('',(#13311,#13312,#13313));
#3333=EDGE_LOOP('',(#13314,#13315,#13316,#13317));
#3334=EDGE_LOOP('',(#13318,#13319,#13320));
#3335=EDGE_LOOP('',(#13321,#13322,#13323,#13324));
#3336=EDGE_LOOP('',(#13325,#13326,#13327));
#3337=EDGE_LOOP('',(#13328,#13329,#13330,#13331));
#3338=EDGE_LOOP('',(#13332,#13333,#13334,#13335));
#3339=EDGE_LOOP('',(#13336,#13337,#13338,#13339));
#3340=EDGE_LOOP('',(#13340,#13341,#13342,#13343));
#3341=EDGE_LOOP('',(#13344,#13345,#13346,#13347));
#3342=EDGE_LOOP('',(#13348,#13349,#13350));
#3343=EDGE_LOOP('',(#13351,#13352,#13353,#13354));
#3344=EDGE_LOOP('',(#13355,#13356,#13357));
#3345=EDGE_LOOP('',(#13358,#13359,#13360,#13361));
#3346=EDGE_LOOP('',(#13362,#13363,#13364));
#3347=EDGE_LOOP('',(#13365,#13366,#13367,#13368));
#3348=EDGE_LOOP('',(#13369,#13370,#13371));
#3349=EDGE_LOOP('',(#13372,#13373,#13374,#13375));
#3350=EDGE_LOOP('',(#13376,#13377,#13378));
#3351=EDGE_LOOP('',(#13379,#13380,#13381,#13382));
#3352=EDGE_LOOP('',(#13383,#13384,#13385));
#3353=EDGE_LOOP('',(#13386,#13387,#13388,#13389));
#3354=EDGE_LOOP('',(#13390,#13391,#13392));
#3355=EDGE_LOOP('',(#13393,#13394,#13395,#13396));
#3356=EDGE_LOOP('',(#13397,#13398,#13399));
#3357=EDGE_LOOP('',(#13400,#13401,#13402,#13403));
#3358=EDGE_LOOP('',(#13404,#13405,#13406));
#3359=EDGE_LOOP('',(#13407,#13408,#13409,#13410));
#3360=EDGE_LOOP('',(#13411,#13412,#13413));
#3361=EDGE_LOOP('',(#13414,#13415,#13416,#13417));
#3362=EDGE_LOOP('',(#13418,#13419,#13420));
#3363=EDGE_LOOP('',(#13421,#13422,#13423,#13424));
#3364=EDGE_LOOP('',(#13425,#13426,#13427));
#3365=EDGE_LOOP('',(#13428,#13429,#13430,#13431));
#3366=EDGE_LOOP('',(#13432,#13433,#13434));
#3367=EDGE_LOOP('',(#13435,#13436,#13437,#13438));
#3368=EDGE_LOOP('',(#13439,#13440,#13441));
#3369=EDGE_LOOP('',(#13442,#13443,#13444,#13445));
#3370=EDGE_LOOP('',(#13446,#13447,#13448));
#3371=EDGE_LOOP('',(#13449,#13450,#13451,#13452));
#3372=EDGE_LOOP('',(#13453,#13454,#13455));
#3373=EDGE_LOOP('',(#13456,#13457,#13458,#13459));
#3374=EDGE_LOOP('',(#13460,#13461,#13462));
#3375=EDGE_LOOP('',(#13463,#13464,#13465,#13466));
#3376=EDGE_LOOP('',(#13467,#13468,#13469));
#3377=EDGE_LOOP('',(#13470,#13471,#13472,#13473));
#3378=EDGE_LOOP('',(#13474,#13475,#13476));
#3379=EDGE_LOOP('',(#13477,#13478,#13479,#13480));
#3380=EDGE_LOOP('',(#13481,#13482,#13483));
#3381=EDGE_LOOP('',(#13484,#13485,#13486,#13487));
#3382=EDGE_LOOP('',(#13488,#13489,#13490));
#3383=EDGE_LOOP('',(#13491,#13492,#13493,#13494));
#3384=EDGE_LOOP('',(#13495,#13496,#13497));
#3385=EDGE_LOOP('',(#13498,#13499,#13500,#13501));
#3386=EDGE_LOOP('',(#13502,#13503,#13504));
#3387=EDGE_LOOP('',(#13505,#13506,#13507,#13508));
#3388=EDGE_LOOP('',(#13509,#13510,#13511));
#3389=EDGE_LOOP('',(#13512,#13513,#13514,#13515));
#3390=EDGE_LOOP('',(#13516,#13517,#13518));
#3391=EDGE_LOOP('',(#13519,#13520,#13521,#13522));
#3392=EDGE_LOOP('',(#13523,#13524,#13525));
#3393=EDGE_LOOP('',(#13526,#13527,#13528,#13529));
#3394=EDGE_LOOP('',(#13530,#13531,#13532));
#3395=EDGE_LOOP('',(#13533,#13534,#13535,#13536));
#3396=EDGE_LOOP('',(#13537,#13538,#13539));
#3397=EDGE_LOOP('',(#13540,#13541,#13542,#13543));
#3398=EDGE_LOOP('',(#13544,#13545,#13546));
#3399=EDGE_LOOP('',(#13547,#13548,#13549,#13550));
#3400=EDGE_LOOP('',(#13551,#13552,#13553));
#3401=EDGE_LOOP('',(#13554,#13555,#13556,#13557));
#3402=EDGE_LOOP('',(#13558,#13559,#13560));
#3403=EDGE_LOOP('',(#13561,#13562,#13563,#13564));
#3404=EDGE_LOOP('',(#13565,#13566,#13567));
#3405=EDGE_LOOP('',(#13568,#13569,#13570,#13571));
#3406=EDGE_LOOP('',(#13572,#13573,#13574));
#3407=EDGE_LOOP('',(#13575,#13576,#13577,#13578));
#3408=EDGE_LOOP('',(#13579,#13580,#13581));
#3409=EDGE_LOOP('',(#13582,#13583,#13584,#13585));
#3410=EDGE_LOOP('',(#13586,#13587,#13588));
#3411=EDGE_LOOP('',(#13589,#13590,#13591,#13592));
#3412=EDGE_LOOP('',(#13593,#13594,#13595));
#3413=EDGE_LOOP('',(#13596,#13597,#13598,#13599));
#3414=EDGE_LOOP('',(#13600,#13601,#13602,#13603));
#3415=EDGE_LOOP('',(#13604,#13605,#13606,#13607));
#3416=EDGE_LOOP('',(#13608,#13609,#13610,#13611));
#3417=EDGE_LOOP('',(#13612,#13613,#13614,#13615));
#3418=EDGE_LOOP('',(#13616,#13617,#13618,#13619));
#3419=EDGE_LOOP('',(#13620,#13621,#13622,#13623,#13624,#13625));
#3420=EDGE_LOOP('',(#13626));
#3421=EDGE_LOOP('',(#13627,#13628,#13629,#13630,#13631,#13632));
#3422=EDGE_LOOP('',(#13633,#13634,#13635,#13636));
#3423=EDGE_LOOP('',(#13637));
#3424=EDGE_LOOP('',(#13638,#13639,#13640,#13641));
#3425=EDGE_LOOP('',(#13642,#13643,#13644,#13645,#13646,#13647,#13648,#13649,
#13650,#13651,#13652,#13653));
#3426=EDGE_LOOP('',(#13654,#13655,#13656,#13657));
#3427=EDGE_LOOP('',(#13658,#13659,#13660,#13661));
#3428=EDGE_LOOP('',(#13662,#13663,#13664,#13665));
#3429=EDGE_LOOP('',(#13666,#13667,#13668,#13669));
#3430=EDGE_LOOP('',(#13670,#13671,#13672,#13673));
#3431=EDGE_LOOP('',(#13674,#13675,#13676,#13677));
#3432=EDGE_LOOP('',(#13678,#13679,#13680,#13681));
#3433=EDGE_LOOP('',(#13682,#13683,#13684,#13685));
#3434=EDGE_LOOP('',(#13686,#13687,#13688,#13689));
#3435=EDGE_LOOP('',(#13690,#13691,#13692,#13693));
#3436=EDGE_LOOP('',(#13694,#13695,#13696,#13697));
#3437=EDGE_LOOP('',(#13698,#13699,#13700,#13701));
#3438=EDGE_LOOP('',(#13702,#13703,#13704,#13705));
#3439=EDGE_LOOP('',(#13706,#13707,#13708,#13709));
#3440=EDGE_LOOP('',(#13710,#13711,#13712,#13713));
#3441=EDGE_LOOP('',(#13714,#13715,#13716,#13717));
#3442=EDGE_LOOP('',(#13718,#13719,#13720,#13721));
#3443=EDGE_LOOP('',(#13722,#13723,#13724,#13725));
#3444=EDGE_LOOP('',(#13726,#13727,#13728,#13729));
#3445=EDGE_LOOP('',(#13730,#13731,#13732,#13733));
#3446=EDGE_LOOP('',(#13734,#13735,#13736,#13737));
#3447=EDGE_LOOP('',(#13738,#13739,#13740,#13741));
#3448=EDGE_LOOP('',(#13742,#13743,#13744,#13745));
#3449=EDGE_LOOP('',(#13746,#13747,#13748,#13749));
#3450=EDGE_LOOP('',(#13750,#13751,#13752,#13753));
#3451=EDGE_LOOP('',(#13754,#13755,#13756,#13757));
#3452=EDGE_LOOP('',(#13758,#13759,#13760,#13761));
#3453=EDGE_LOOP('',(#13762,#13763,#13764,#13765));
#3454=EDGE_LOOP('',(#13766,#13767,#13768,#13769));
#3455=EDGE_LOOP('',(#13770,#13771,#13772,#13773));
#3456=EDGE_LOOP('',(#13774,#13775,#13776,#13777));
#3457=EDGE_LOOP('',(#13778,#13779,#13780,#13781));
#3458=EDGE_LOOP('',(#13782,#13783,#13784,#13785));
#3459=EDGE_LOOP('',(#13786,#13787,#13788,#13789));
#3460=EDGE_LOOP('',(#13790,#13791,#13792,#13793));
#3461=EDGE_LOOP('',(#13794,#13795,#13796,#13797));
#3462=EDGE_LOOP('',(#13798));
#3463=EDGE_LOOP('',(#13799,#13800,#13801,#13802,#13803,#13804));
#3464=EDGE_LOOP('',(#13805,#13806,#13807,#13808));
#3465=EDGE_LOOP('',(#13809,#13810,#13811,#13812));
#3466=EDGE_LOOP('',(#13813,#13814,#13815,#13816));
#3467=EDGE_LOOP('',(#13817,#13818,#13819,#13820));
#3468=EDGE_LOOP('',(#13821,#13822,#13823,#13824));
#3469=EDGE_LOOP('',(#13825,#13826,#13827,#13828));
#3470=EDGE_LOOP('',(#13829,#13830,#13831,#13832));
#3471=EDGE_LOOP('',(#13833,#13834,#13835));
#3472=EDGE_LOOP('',(#13836,#13837,#13838,#13839,#13840));
#3473=EDGE_LOOP('',(#13841,#13842,#13843,#13844));
#3474=EDGE_LOOP('',(#13845,#13846,#13847,#13848));
#3475=EDGE_LOOP('',(#13849,#13850,#13851,#13852));
#3476=EDGE_LOOP('',(#13853,#13854,#13855,#13856));
#3477=EDGE_LOOP('',(#13857,#13858,#13859,#13860));
#3478=EDGE_LOOP('',(#13861,#13862,#13863));
#3479=EDGE_LOOP('',(#13864,#13865,#13866,#13867));
#3480=EDGE_LOOP('',(#13868,#13869,#13870));
#3481=EDGE_LOOP('',(#13871,#13872,#13873,#13874));
#3482=EDGE_LOOP('',(#13875,#13876,#13877,#13878));
#3483=EDGE_LOOP('',(#13879,#13880,#13881));
#3484=EDGE_LOOP('',(#13882,#13883,#13884,#13885));
#3485=EDGE_LOOP('',(#13886,#13887,#13888));
#3486=EDGE_LOOP('',(#13889,#13890,#13891,#13892));
#3487=EDGE_LOOP('',(#13893,#13894,#13895,#13896));
#3488=EDGE_LOOP('',(#13897,#13898,#13899));
#3489=EDGE_LOOP('',(#13900,#13901,#13902,#13903));
#3490=EDGE_LOOP('',(#13904,#13905,#13906));
#3491=EDGE_LOOP('',(#13907,#13908,#13909,#13910));
#3492=EDGE_LOOP('',(#13911,#13912,#13913,#13914));
#3493=EDGE_LOOP('',(#13915,#13916,#13917,#13918));
#3494=EDGE_LOOP('',(#13919,#13920,#13921,#13922));
#3495=EDGE_LOOP('',(#13923,#13924,#13925,#13926));
#3496=EDGE_LOOP('',(#13927,#13928,#13929,#13930));
#3497=EDGE_LOOP('',(#13931,#13932,#13933,#13934));
#3498=EDGE_LOOP('',(#13935,#13936,#13937,#13938));
#3499=EDGE_LOOP('',(#13939,#13940,#13941,#13942,#13943,#13944));
#3500=EDGE_LOOP('',(#13945,#13946,#13947,#13948,#13949,#13950));
#3501=EDGE_LOOP('',(#13951,#13952,#13953,#13954));
#3502=EDGE_LOOP('',(#13955,#13956,#13957,#13958));
#3503=EDGE_LOOP('',(#13959,#13960,#13961,#13962));
#3504=EDGE_LOOP('',(#13963,#13964,#13965,#13966));
#3505=EDGE_LOOP('',(#13967,#13968,#13969,#13970));
#3506=EDGE_LOOP('',(#13971,#13972,#13973,#13974));
#3507=EDGE_LOOP('',(#13975,#13976,#13977,#13978));
#3508=EDGE_LOOP('',(#13979,#13980,#13981,#13982));
#3509=EDGE_LOOP('',(#13983,#13984,#13985,#13986));
#3510=EDGE_LOOP('',(#13987,#13988,#13989,#13990,#13991,#13992,#13993,#13994,
#13995,#13996,#13997,#13998,#13999,#14000,#14001,#14002,#14003));
#3511=EDGE_LOOP('',(#14004,#14005,#14006,#14007,#14008));
#3512=EDGE_LOOP('',(#14009,#14010,#14011,#14012));
#3513=EDGE_LOOP('',(#14013,#14014,#14015,#14016,#14017,#14018,#14019,#14020,
#14021,#14022,#14023,#14024,#14025,#14026,#14027,#14028,#14029,#14030));
#3514=EDGE_LOOP('',(#14031,#14032,#14033,#14034,#14035));
#3515=EDGE_LOOP('',(#14036));
#3516=EDGE_LOOP('',(#14037,#14038,#14039,#14040));
#3517=EDGE_LOOP('',(#14041,#14042,#14043,#14044));
#3518=EDGE_LOOP('',(#14045,#14046,#14047,#14048));
#3519=EDGE_LOOP('',(#14049,#14050,#14051,#14052,#14053,#14054));
#3520=EDGE_LOOP('',(#14055,#14056,#14057,#14058));
#3521=EDGE_LOOP('',(#14059,#14060,#14061,#14062));
#3522=EDGE_LOOP('',(#14063,#14064,#14065,#14066));
#3523=EDGE_LOOP('',(#14067));
#3524=EDGE_LOOP('',(#14068,#14069,#14070,#14071,#14072,#14073,#14074,#14075,
#14076,#14077,#14078,#14079));
#3525=EDGE_LOOP('',(#14080));
#3526=EDGE_LOOP('',(#14081));
#3527=EDGE_LOOP('',(#14082,#14083,#14084,#14085));
#3528=EDGE_LOOP('',(#14086));
#3529=EDGE_LOOP('',(#14087,#14088,#14089,#14090,#14091,#14092));
#3530=EDGE_LOOP('',(#14093,#14094,#14095,#14096));
#3531=EDGE_LOOP('',(#14097,#14098,#14099,#14100));
#3532=LINE('',#20896,#4601);
#3533=LINE('',#20900,#4602);
#3534=LINE('',#20922,#4603);
#3535=LINE('',#20927,#4604);
#3536=LINE('',#20931,#4605);
#3537=LINE('',#20935,#4606);
#3538=LINE('',#20940,#4607);
#3539=LINE('',#20945,#4608);
#3540=LINE('',#20952,#4609);
#3541=LINE('',#20971,#4610);
#3542=LINE('',#20976,#4611);
#3543=LINE('',#20980,#4612);
#3544=LINE('',#20984,#4613);
#3545=LINE('',#20989,#4614);
#3546=LINE('',#20992,#4615);
#3547=LINE('',#20996,#4616);
#3548=LINE('',#21018,#4617);
#3549=LINE('',#21023,#4618);
#3550=LINE('',#21027,#4619);
#3551=LINE('',#21031,#4620);
#3552=LINE('',#21035,#4621);
#3553=LINE('',#21047,#4622);
#3554=LINE('',#21051,#4623);
#3555=LINE('',#21055,#4624);
#3556=LINE('',#21059,#4625);
#3557=LINE('',#21063,#4626);
#3558=LINE('',#21067,#4627);
#3559=LINE('',#21071,#4628);
#3560=LINE('',#21095,#4629);
#3561=LINE('',#21098,#4630);
#3562=LINE('',#21101,#4631);
#3563=LINE('',#21103,#4632);
#3564=LINE('',#21105,#4633);
#3565=LINE('',#21107,#4634);
#3566=LINE('',#21109,#4635);
#3567=LINE('',#21111,#4636);
#3568=LINE('',#21129,#4637);
#3569=LINE('',#21132,#4638);
#3570=LINE('',#21135,#4639);
#3571=LINE('',#21148,#4640);
#3572=LINE('',#21161,#4641);
#3573=LINE('',#21163,#4642);
#3574=LINE('',#21164,#4643);
#3575=LINE('',#21166,#4644);
#3576=LINE('',#21168,#4645);
#3577=LINE('',#21169,#4646);
#3578=LINE('',#21184,#4647);
#3579=LINE('',#21207,#4648);
#3580=LINE('',#21210,#4649);
#3581=LINE('',#21222,#4650);
#3582=LINE('',#21226,#4651);
#3583=LINE('',#21296,#4652);
#3584=LINE('',#21299,#4653);
#3585=LINE('',#21302,#4654);
#3586=LINE('',#21304,#4655);
#3587=LINE('',#21306,#4656);
#3588=LINE('',#21308,#4657);
#3589=LINE('',#21309,#4658);
#3590=LINE('',#21324,#4659);
#3591=LINE('',#21327,#4660);
#3592=LINE('',#21330,#4661);
#3593=LINE('',#21343,#4662);
#3594=LINE('',#21356,#4663);
#3595=LINE('',#21358,#4664);
#3596=LINE('',#21360,#4665);
#3597=LINE('',#21362,#4666);
#3598=LINE('',#21363,#4667);
#3599=LINE('',#21364,#4668);
#3600=LINE('',#21379,#4669);
#3601=LINE('',#21399,#4670);
#3602=LINE('',#21411,#4671);
#3603=LINE('',#21415,#4672);
#3604=LINE('',#21466,#4673);
#3605=LINE('',#21472,#4674);
#3606=LINE('',#21476,#4675);
#3607=LINE('',#21480,#4676);
#3608=LINE('',#21483,#4677);
#3609=LINE('',#21489,#4678);
#3610=LINE('',#21522,#4679);
#3611=LINE('',#21542,#4680);
#3612=LINE('',#21565,#4681);
#3613=LINE('',#21567,#4682);
#3614=LINE('',#21570,#4683);
#3615=LINE('',#21573,#4684);
#3616=LINE('',#21575,#4685);
#3617=LINE('',#21581,#4686);
#3618=LINE('',#21587,#4687);
#3619=LINE('',#21589,#4688);
#3620=LINE('',#21591,#4689);
#3621=LINE('',#21597,#4690);
#3622=LINE('',#21609,#4691);
#3623=LINE('',#21612,#4692);
#3624=LINE('',#21620,#4693);
#3625=LINE('',#21630,#4694);
#3626=LINE('',#21632,#4695);
#3627=LINE('',#21636,#4696);
#3628=LINE('',#21644,#4697);
#3629=LINE('',#21648,#4698);
#3630=LINE('',#21656,#4699);
#3631=LINE('',#21689,#4700);
#3632=LINE('',#22595,#4701);
#3633=LINE('',#22604,#4702);
#3634=LINE('',#22611,#4703);
#3635=LINE('',#22618,#4704);
#3636=LINE('',#22631,#4705);
#3637=LINE('',#22640,#4706);
#3638=LINE('',#22646,#4707);
#3639=LINE('',#22653,#4708);
#3640=LINE('',#22657,#4709);
#3641=LINE('',#22661,#4710);
#3642=LINE('',#22664,#4711);
#3643=LINE('',#22667,#4712);
#3644=LINE('',#22739,#4713);
#3645=LINE('',#22744,#4714);
#3646=LINE('',#22795,#4715);
#3647=LINE('',#22810,#4716);
#3648=LINE('',#22850,#4717);
#3649=LINE('',#22854,#4718);
#3650=LINE('',#22914,#4719);
#3651=LINE('',#22925,#4720);
#3652=LINE('',#22984,#4721);
#3653=LINE('',#22985,#4722);
#3654=LINE('',#23005,#4723);
#3655=LINE('',#23009,#4724);
#3656=LINE('',#23013,#4725);
#3657=LINE('',#23017,#4726);
#3658=LINE('',#23020,#4727);
#3659=LINE('',#23071,#4728);
#3660=LINE('',#23086,#4729);
#3661=LINE('',#23131,#4730);
#3662=LINE('',#23135,#4731);
#3663=LINE('',#23195,#4732);
#3664=LINE('',#23206,#4733);
#3665=LINE('',#23265,#4734);
#3666=LINE('',#23266,#4735);
#3667=LINE('',#23271,#4736);
#3668=LINE('',#23275,#4737);
#3669=LINE('',#23279,#4738);
#3670=LINE('',#23283,#4739);
#3671=LINE('',#23327,#4740);
#3672=LINE('',#23340,#4741);
#3673=LINE('',#23377,#4742);
#3674=LINE('',#23382,#4743);
#3675=LINE('',#23432,#4744);
#3676=LINE('',#23434,#4745);
#3677=LINE('',#23483,#4746);
#3678=LINE('',#23487,#4747);
#3679=LINE('',#23490,#4748);
#3680=LINE('',#23517,#4749);
#3681=LINE('',#23526,#4750);
#3682=LINE('',#23560,#4751);
#3683=LINE('',#23564,#4752);
#3684=LINE('',#23644,#4753);
#3685=LINE('',#23660,#4754);
#3686=LINE('',#23729,#4755);
#3687=LINE('',#23730,#4756);
#3688=LINE('',#23735,#4757);
#3689=LINE('',#23739,#4758);
#3690=LINE('',#23832,#4759);
#3691=LINE('',#23896,#4760);
#3692=LINE('',#23960,#4761);
#3693=LINE('',#23980,#4762);
#3694=LINE('',#24124,#4763);
#3695=LINE('',#24140,#4764);
#3696=LINE('',#24218,#4765);
#3697=LINE('',#24226,#4766);
#3698=LINE('',#24228,#4767);
#3699=LINE('',#24230,#4768);
#3700=LINE('',#24238,#4769);
#3701=LINE('',#24240,#4770);
#3702=LINE('',#24241,#4771);
#3703=LINE('',#24246,#4772);
#3704=LINE('',#24251,#4773);
#3705=LINE('',#24253,#4774);
#3706=LINE('',#24255,#4775);
#3707=LINE('',#24256,#4776);
#3708=LINE('',#24267,#4777);
#3709=LINE('',#24271,#4778);
#3710=LINE('',#24275,#4779);
#3711=LINE('',#24279,#4780);
#3712=LINE('',#24283,#4781);
#3713=LINE('',#24287,#4782);
#3714=LINE('',#24291,#4783);
#3715=LINE('',#24295,#4784);
#3716=LINE('',#24299,#4785);
#3717=LINE('',#24470,#4786);
#3718=LINE('',#24476,#4787);
#3719=LINE('',#24492,#4788);
#3720=LINE('',#24501,#4789);
#3721=LINE('',#24519,#4790);
#3722=LINE('',#24520,#4791);
#3723=LINE('',#24524,#4792);
#3724=LINE('',#24530,#4793);
#3725=LINE('',#24549,#4794);
#3726=LINE('',#24551,#4795);
#3727=LINE('',#24552,#4796);
#3728=LINE('',#24580,#4797);
#3729=LINE('',#24581,#4798);
#3730=LINE('',#24584,#4799);
#3731=LINE('',#24586,#4800);
#3732=LINE('',#24608,#4801);
#3733=LINE('',#24609,#4802);
#3734=LINE('',#24611,#4803);
#3735=LINE('',#24613,#4804);
#3736=LINE('',#24619,#4805);
#3737=LINE('',#24624,#4806);
#3738=LINE('',#24644,#4807);
#3739=LINE('',#24653,#4808);
#3740=LINE('',#25148,#4809);
#3741=LINE('',#25152,#4810);
#3742=LINE('',#25154,#4811);
#3743=LINE('',#25245,#4812);
#3744=LINE('',#25251,#4813);
#3745=LINE('',#25253,#4814);
#3746=LINE('',#25255,#4815);
#3747=LINE('',#25258,#4816);
#3748=LINE('',#25260,#4817);
#3749=LINE('',#25270,#4818);
#3750=LINE('',#25288,#4819);
#3751=LINE('',#25289,#4820);
#3752=LINE('',#25293,#4821);
#3753=LINE('',#25294,#4822);
#3754=LINE('',#25296,#4823);
#3755=LINE('',#25298,#4824);
#3756=LINE('',#25311,#4825);
#3757=LINE('',#25313,#4826);
#3758=LINE('',#25334,#4827);
#3759=LINE('',#25337,#4828);
#3760=LINE('',#25341,#4829);
#3761=LINE('',#25366,#4830);
#3762=LINE('',#25369,#4831);
#3763=LINE('',#25376,#4832);
#3764=LINE('',#25378,#4833);
#3765=LINE('',#25382,#4834);
#3766=LINE('',#25384,#4835);
#3767=LINE('',#25386,#4836);
#3768=LINE('',#25402,#4837);
#3769=LINE('',#25408,#4838);
#3770=LINE('',#25417,#4839);
#3771=LINE('',#25420,#4840);
#3772=LINE('',#25423,#4841);
#3773=LINE('',#25425,#4842);
#3774=LINE('',#25426,#4843);
#3775=LINE('',#25433,#4844);
#3776=LINE('',#25442,#4845);
#3777=LINE('',#25445,#4846);
#3778=LINE('',#25453,#4847);
#3779=LINE('',#25454,#4848);
#3780=LINE('',#25461,#4849);
#3781=LINE('',#25464,#4850);
#3782=LINE('',#25466,#4851);
#3783=LINE('',#25475,#4852);
#3784=LINE('',#25494,#4853);
#3785=LINE('',#25498,#4854);
#3786=LINE('',#25499,#4855);
#3787=LINE('',#25503,#4856);
#3788=LINE('',#25507,#4857);
#3789=LINE('',#25509,#4858);
#3790=LINE('',#25514,#4859);
#3791=LINE('',#25515,#4860);
#3792=LINE('',#25517,#4861);
#3793=LINE('',#25520,#4862);
#3794=LINE('',#25522,#4863);
#3795=LINE('',#25523,#4864);
#3796=LINE('',#25526,#4865);
#3797=LINE('',#25527,#4866);
#3798=LINE('',#25535,#4867);
#3799=LINE('',#25537,#4868);
#3800=LINE('',#25540,#4869);
#3801=LINE('',#25541,#4870);
#3802=LINE('',#25544,#4871);
#3803=LINE('',#25545,#4872);
#3804=LINE('',#25547,#4873);
#3805=LINE('',#25567,#4874);
#3806=LINE('',#25571,#4875);
#3807=LINE('',#25576,#4876);
#3808=LINE('',#25580,#4877);
#3809=LINE('',#25585,#4878);
#3810=LINE('',#25589,#4879);
#3811=LINE('',#25594,#4880);
#3812=LINE('',#25598,#4881);
#3813=LINE('',#25603,#4882);
#3814=LINE('',#25607,#4883);
#3815=LINE('',#25612,#4884);
#3816=LINE('',#25616,#4885);
#3817=LINE('',#25621,#4886);
#3818=LINE('',#25625,#4887);
#3819=LINE('',#25629,#4888);
#3820=LINE('',#25636,#4889);
#3821=LINE('',#25639,#4890);
#3822=LINE('',#25642,#4891);
#3823=LINE('',#25644,#4892);
#3824=LINE('',#25645,#4893);
#3825=LINE('',#25651,#4894);
#3826=LINE('',#25657,#4895);
#3827=LINE('',#25660,#4896);
#3828=LINE('',#25663,#4897);
#3829=LINE('',#25665,#4898);
#3830=LINE('',#25666,#4899);
#3831=LINE('',#25672,#4900);
#3832=LINE('',#25678,#4901);
#3833=LINE('',#25681,#4902);
#3834=LINE('',#25684,#4903);
#3835=LINE('',#25686,#4904);
#3836=LINE('',#25687,#4905);
#3837=LINE('',#25693,#4906);
#3838=LINE('',#25699,#4907);
#3839=LINE('',#25702,#4908);
#3840=LINE('',#25705,#4909);
#3841=LINE('',#25707,#4910);
#3842=LINE('',#25708,#4911);
#3843=LINE('',#25714,#4912);
#3844=LINE('',#25731,#4913);
#3845=LINE('',#25739,#4914);
#3846=LINE('',#25745,#4915);
#3847=LINE('',#25751,#4916);
#3848=LINE('',#25759,#4917);
#3849=LINE('',#25765,#4918);
#3850=LINE('',#25783,#4919);
#3851=LINE('',#25785,#4920);
#3852=LINE('',#25787,#4921);
#3853=LINE('',#25789,#4922);
#3854=LINE('',#25795,#4923);
#3855=LINE('',#25796,#4924);
#3856=LINE('',#25803,#4925);
#3857=LINE('',#25805,#4926);
#3858=LINE('',#25806,#4927);
#3859=LINE('',#25810,#4928);
#3860=LINE('',#25816,#4929);
#3861=LINE('',#25824,#4930);
#3862=LINE('',#25830,#4931);
#3863=LINE('',#25848,#4932);
#3864=LINE('',#25850,#4933);
#3865=LINE('',#25852,#4934);
#3866=LINE('',#25854,#4935);
#3867=LINE('',#25860,#4936);
#3868=LINE('',#25861,#4937);
#3869=LINE('',#25868,#4938);
#3870=LINE('',#25870,#4939);
#3871=LINE('',#25871,#4940);
#3872=LINE('',#25875,#4941);
#3873=LINE('',#25881,#4942);
#3874=LINE('',#25889,#4943);
#3875=LINE('',#25895,#4944);
#3876=LINE('',#25913,#4945);
#3877=LINE('',#25915,#4946);
#3878=LINE('',#25917,#4947);
#3879=LINE('',#25919,#4948);
#3880=LINE('',#25925,#4949);
#3881=LINE('',#25926,#4950);
#3882=LINE('',#25933,#4951);
#3883=LINE('',#25935,#4952);
#3884=LINE('',#25936,#4953);
#3885=LINE('',#25940,#4954);
#3886=LINE('',#25946,#4955);
#3887=LINE('',#25954,#4956);
#3888=LINE('',#25960,#4957);
#3889=LINE('',#25978,#4958);
#3890=LINE('',#25980,#4959);
#3891=LINE('',#25982,#4960);
#3892=LINE('',#25984,#4961);
#3893=LINE('',#25990,#4962);
#3894=LINE('',#25991,#4963);
#3895=LINE('',#25998,#4964);
#3896=LINE('',#26000,#4965);
#3897=LINE('',#26001,#4966);
#3898=LINE('',#26009,#4967);
#3899=LINE('',#26014,#4968);
#3900=LINE('',#26021,#4969);
#3901=LINE('',#26023,#4970);
#3902=LINE('',#26025,#4971);
#3903=LINE('',#26027,#4972);
#3904=LINE('',#26034,#4973);
#3905=LINE('',#26040,#4974);
#3906=LINE('',#26058,#4975);
#3907=LINE('',#26060,#4976);
#3908=LINE('',#26062,#4977);
#3909=LINE('',#26063,#4978);
#3910=LINE('',#26080,#4979);
#3911=LINE('',#26084,#4980);
#3912=LINE('',#26088,#4981);
#3913=LINE('',#26092,#4982);
#3914=LINE('',#26096,#4983);
#3915=LINE('',#26100,#4984);
#3916=LINE('',#26104,#4985);
#3917=LINE('',#26107,#4986);
#3918=LINE('',#26115,#4987);
#3919=LINE('',#26119,#4988);
#3920=LINE('',#26123,#4989);
#3921=LINE('',#26127,#4990);
#3922=LINE('',#26131,#4991);
#3923=LINE('',#26135,#4992);
#3924=LINE('',#26139,#4993);
#3925=LINE('',#26143,#4994);
#3926=LINE('',#26147,#4995);
#3927=LINE('',#26151,#4996);
#3928=LINE('',#26162,#4997);
#3929=LINE('',#26179,#4998);
#3930=LINE('',#26181,#4999);
#3931=LINE('',#26183,#5000);
#3932=LINE('',#26184,#5001);
#3933=LINE('',#26187,#5002);
#3934=LINE('',#26188,#5003);
#3935=LINE('',#26195,#5004);
#3936=LINE('',#26197,#5005);
#3937=LINE('',#26198,#5006);
#3938=LINE('',#26202,#5007);
#3939=LINE('',#26216,#5008);
#3940=LINE('',#26233,#5009);
#3941=LINE('',#26235,#5010);
#3942=LINE('',#26237,#5011);
#3943=LINE('',#26239,#5012);
#3944=LINE('',#26245,#5013);
#3945=LINE('',#26246,#5014);
#3946=LINE('',#26253,#5015);
#3947=LINE('',#26255,#5016);
#3948=LINE('',#26256,#5017);
#3949=LINE('',#26260,#5018);
#3950=LINE('',#26262,#5019);
#3951=LINE('',#26264,#5020);
#3952=LINE('',#26265,#5021);
#3953=LINE('',#26268,#5022);
#3954=LINE('',#26270,#5023);
#3955=LINE('',#26271,#5024);
#3956=LINE('',#26275,#5025);
#3957=LINE('',#26277,#5026);
#3958=LINE('',#26279,#5027);
#3959=LINE('',#26280,#5028);
#3960=LINE('',#26283,#5029);
#3961=LINE('',#26285,#5030);
#3962=LINE('',#26286,#5031);
#3963=LINE('',#26290,#5032);
#3964=LINE('',#26292,#5033);
#3965=LINE('',#26294,#5034);
#3966=LINE('',#26295,#5035);
#3967=LINE('',#26298,#5036);
#3968=LINE('',#26300,#5037);
#3969=LINE('',#26301,#5038);
#3970=LINE('',#26305,#5039);
#3971=LINE('',#26307,#5040);
#3972=LINE('',#26309,#5041);
#3973=LINE('',#26310,#5042);
#3974=LINE('',#26313,#5043);
#3975=LINE('',#26315,#5044);
#3976=LINE('',#26316,#5045);
#3977=LINE('',#26320,#5046);
#3978=LINE('',#26322,#5047);
#3979=LINE('',#26324,#5048);
#3980=LINE('',#26325,#5049);
#3981=LINE('',#26328,#5050);
#3982=LINE('',#26330,#5051);
#3983=LINE('',#26331,#5052);
#3984=LINE('',#26333,#5053);
#3985=LINE('',#26334,#5054);
#3986=LINE('',#26337,#5055);
#3987=LINE('',#26338,#5056);
#3988=LINE('',#26341,#5057);
#3989=LINE('',#26342,#5058);
#3990=LINE('',#26344,#5059);
#3991=LINE('',#26346,#5060);
#3992=LINE('',#26347,#5061);
#3993=LINE('',#26350,#5062);
#3994=LINE('',#26351,#5063);
#3995=LINE('',#26354,#5064);
#3996=LINE('',#26355,#5065);
#3997=LINE('',#26358,#5066);
#3998=LINE('',#26359,#5067);
#3999=LINE('',#26364,#5068);
#4000=LINE('',#26378,#5069);
#4001=LINE('',#26394,#5070);
#4002=LINE('',#26396,#5071);
#4003=LINE('',#26401,#5072);
#4004=LINE('',#26407,#5073);
#4005=LINE('',#26411,#5074);
#4006=LINE('',#26425,#5075);
#4007=LINE('',#26441,#5076);
#4008=LINE('',#26443,#5077);
#4009=LINE('',#26448,#5078);
#4010=LINE('',#26454,#5079);
#4011=LINE('',#26458,#5080);
#4012=LINE('',#26472,#5081);
#4013=LINE('',#26488,#5082);
#4014=LINE('',#26490,#5083);
#4015=LINE('',#26495,#5084);
#4016=LINE('',#26501,#5085);
#4017=LINE('',#26505,#5086);
#4018=LINE('',#26519,#5087);
#4019=LINE('',#26535,#5088);
#4020=LINE('',#26537,#5089);
#4021=LINE('',#26542,#5090);
#4022=LINE('',#26548,#5091);
#4023=LINE('',#26552,#5092);
#4024=LINE('',#26566,#5093);
#4025=LINE('',#26582,#5094);
#4026=LINE('',#26583,#5095);
#4027=LINE('',#26589,#5096);
#4028=LINE('',#26603,#5097);
#4029=LINE('',#26605,#5098);
#4030=LINE('',#26607,#5099);
#4031=LINE('',#26608,#5100);
#4032=LINE('',#26611,#5101);
#4033=LINE('',#26613,#5102);
#4034=LINE('',#26614,#5103);
#4035=LINE('',#26617,#5104);
#4036=LINE('',#26628,#5105);
#4037=LINE('',#26644,#5106);
#4038=LINE('',#26645,#5107);
#4039=LINE('',#26651,#5108);
#4040=LINE('',#26658,#5109);
#4041=LINE('',#26662,#5110);
#4042=LINE('',#26665,#5111);
#4043=LINE('',#26677,#5112);
#4044=LINE('',#26684,#5113);
#4045=LINE('',#26686,#5114);
#4046=LINE('',#26687,#5115);
#4047=LINE('',#26690,#5116);
#4048=LINE('',#26692,#5117);
#4049=LINE('',#26693,#5118);
#4050=LINE('',#26696,#5119);
#4051=LINE('',#26698,#5120);
#4052=LINE('',#26699,#5121);
#4053=LINE('',#26702,#5122);
#4054=LINE('',#26726,#5123);
#4055=LINE('',#26733,#5124);
#4056=LINE('',#26740,#5125);
#4057=LINE('',#26744,#5126);
#4058=LINE('',#26750,#5127);
#4059=LINE('',#26752,#5128);
#4060=LINE('',#26754,#5129);
#4061=LINE('',#26756,#5130);
#4062=LINE('',#26758,#5131);
#4063=LINE('',#26759,#5132);
#4064=LINE('',#26762,#5133);
#4065=LINE('',#26764,#5134);
#4066=LINE('',#26765,#5135);
#4067=LINE('',#26768,#5136);
#4068=LINE('',#26770,#5137);
#4069=LINE('',#26772,#5138);
#4070=LINE('',#26773,#5139);
#4071=LINE('',#26776,#5140);
#4072=LINE('',#26778,#5141);
#4073=LINE('',#26780,#5142);
#4074=LINE('',#26781,#5143);
#4075=LINE('',#26785,#5144);
#4076=LINE('',#26787,#5145);
#4077=LINE('',#26788,#5146);
#4078=LINE('',#26790,#5147);
#4079=LINE('',#26791,#5148);
#4080=LINE('',#26794,#5149);
#4081=LINE('',#26796,#5150);
#4082=LINE('',#26797,#5151);
#4083=LINE('',#26800,#5152);
#4084=LINE('',#26802,#5153);
#4085=LINE('',#26804,#5154);
#4086=LINE('',#26805,#5155);
#4087=LINE('',#26808,#5156);
#4088=LINE('',#26809,#5157);
#4089=LINE('',#26810,#5158);
#4090=LINE('',#26813,#5159);
#4091=LINE('',#26814,#5160);
#4092=LINE('',#26817,#5161);
#4093=LINE('',#26819,#5162);
#4094=LINE('',#26821,#5163);
#4095=LINE('',#26822,#5164);
#4096=LINE('',#26825,#5165);
#4097=LINE('',#26826,#5166);
#4098=LINE('',#26827,#5167);
#4099=LINE('',#26830,#5168);
#4100=LINE('',#26831,#5169);
#4101=LINE('',#26834,#5170);
#4102=LINE('',#26836,#5171);
#4103=LINE('',#26837,#5172);
#4104=LINE('',#26839,#5173);
#4105=LINE('',#26841,#5174);
#4106=LINE('',#26850,#5175);
#4107=LINE('',#26857,#5176);
#4108=LINE('',#26865,#5177);
#4109=LINE('',#26869,#5178);
#4110=LINE('',#26873,#5179);
#4111=LINE('',#26879,#5180);
#4112=LINE('',#26887,#5181);
#4113=LINE('',#26893,#5182);
#4114=LINE('',#26897,#5183);
#4115=LINE('',#26901,#5184);
#4116=LINE('',#26909,#5185);
#4117=LINE('',#26920,#5186);
#4118=LINE('',#26925,#5187);
#4119=LINE('',#26933,#5188);
#4120=LINE('',#26939,#5189);
#4121=LINE('',#26944,#5190);
#4122=LINE('',#26954,#5191);
#4123=LINE('',#26961,#5192);
#4124=LINE('',#26969,#5193);
#4125=LINE('',#26977,#5194);
#4126=LINE('',#26981,#5195);
#4127=LINE('',#26986,#5196);
#4128=LINE('',#26991,#5197);
#4129=LINE('',#26997,#5198);
#4130=LINE('',#27002,#5199);
#4131=LINE('',#27011,#5200);
#4132=LINE('',#27019,#5201);
#4133=LINE('',#27029,#5202);
#4134=LINE('',#27033,#5203);
#4135=LINE('',#27035,#5204);
#4136=LINE('',#27087,#5205);
#4137=LINE('',#27095,#5206);
#4138=LINE('',#27099,#5207);
#4139=LINE('',#27106,#5208);
#4140=LINE('',#27123,#5209);
#4141=LINE('',#27131,#5210);
#4142=LINE('',#27166,#5211);
#4143=LINE('',#27172,#5212);
#4144=LINE('',#27173,#5213);
#4145=LINE('',#27177,#5214);
#4146=LINE('',#27181,#5215);
#4147=LINE('',#27185,#5216);
#4148=LINE('',#27189,#5217);
#4149=LINE('',#27193,#5218);
#4150=LINE('',#27197,#5219);
#4151=LINE('',#27201,#5220);
#4152=LINE('',#27205,#5221);
#4153=LINE('',#27209,#5222);
#4154=LINE('',#27213,#5223);
#4155=LINE('',#27217,#5224);
#4156=LINE('',#27221,#5225);
#4157=LINE('',#27228,#5226);
#4158=LINE('',#27233,#5227);
#4159=LINE('',#27266,#5228);
#4160=LINE('',#27350,#5229);
#4161=LINE('',#27440,#5230);
#4162=LINE('',#27524,#5231);
#4163=LINE('',#27614,#5232);
#4164=LINE('',#27704,#5233);
#4165=LINE('',#27788,#5234);
#4166=LINE('',#27878,#5235);
#4167=LINE('',#27962,#5236);
#4168=LINE('',#28052,#5237);
#4169=LINE('',#28136,#5238);
#4170=LINE('',#28226,#5239);
#4171=LINE('',#28313,#5240);
#4172=LINE('',#28400,#5241);
#4173=LINE('',#28490,#5242);
#4174=LINE('',#28574,#5243);
#4175=LINE('',#28664,#5244);
#4176=LINE('',#28748,#5245);
#4177=LINE('',#28838,#5246);
#4178=LINE('',#28922,#5247);
#4179=LINE('',#29009,#5248);
#4180=LINE('',#29099,#5249);
#4181=LINE('',#29183,#5250);
#4182=LINE('',#29273,#5251);
#4183=LINE('',#29357,#5252);
#4184=LINE('',#29447,#5253);
#4185=LINE('',#29531,#5254);
#4186=LINE('',#29621,#5255);
#4187=LINE('',#29711,#5256);
#4188=LINE('',#29795,#5257);
#4189=LINE('',#29885,#5258);
#4190=LINE('',#29969,#5259);
#4191=LINE('',#30059,#5260);
#4192=LINE('',#30143,#5261);
#4193=LINE('',#30165,#5262);
#4194=LINE('',#30202,#5263);
#4195=LINE('',#30239,#5264);
#4196=LINE('',#30276,#5265);
#4197=LINE('',#30313,#5266);
#4198=LINE('',#30350,#5267);
#4199=LINE('',#30387,#5268);
#4200=LINE('',#30425,#5269);
#4201=LINE('',#30462,#5270);
#4202=LINE('',#30499,#5271);
#4203=LINE('',#30536,#5272);
#4204=LINE('',#30573,#5273);
#4205=LINE('',#30610,#5274);
#4206=LINE('',#30647,#5275);
#4207=LINE('',#30685,#5276);
#4208=LINE('',#30721,#5277);
#4209=LINE('',#30759,#5278);
#4210=LINE('',#30796,#5279);
#4211=LINE('',#30833,#5280);
#4212=LINE('',#30870,#5281);
#4213=LINE('',#30907,#5282);
#4214=LINE('',#30945,#5283);
#4215=LINE('',#30981,#5284);
#4216=LINE('',#31019,#5285);
#4217=LINE('',#31056,#5286);
#4218=LINE('',#31093,#5287);
#4219=LINE('',#31130,#5288);
#4220=LINE('',#31167,#5289);
#4221=LINE('',#31204,#5290);
#4222=LINE('',#31241,#5291);
#4223=LINE('',#31279,#5292);
#4224=LINE('',#31316,#5293);
#4225=LINE('',#31353,#5294);
#4226=LINE('',#35416,#5295);
#4227=LINE('',#35418,#5296);
#4228=LINE('',#35420,#5297);
#4229=LINE('',#35421,#5298);
#4230=LINE('',#35425,#5299);
#4231=LINE('',#35428,#5300);
#4232=LINE('',#35429,#5301);
#4233=LINE('',#35435,#5302);
#4234=LINE('',#35437,#5303);
#4235=LINE('',#35439,#5304);
#4236=LINE('',#35440,#5305);
#4237=LINE('',#35444,#5306);
#4238=LINE('',#35447,#5307);
#4239=LINE('',#35448,#5308);
#4240=LINE('',#35454,#5309);
#4241=LINE('',#35456,#5310);
#4242=LINE('',#35458,#5311);
#4243=LINE('',#35459,#5312);
#4244=LINE('',#35463,#5313);
#4245=LINE('',#35466,#5314);
#4246=LINE('',#35467,#5315);
#4247=LINE('',#35473,#5316);
#4248=LINE('',#35475,#5317);
#4249=LINE('',#35477,#5318);
#4250=LINE('',#35478,#5319);
#4251=LINE('',#35482,#5320);
#4252=LINE('',#35485,#5321);
#4253=LINE('',#35486,#5322);
#4254=LINE('',#35492,#5323);
#4255=LINE('',#35494,#5324);
#4256=LINE('',#35496,#5325);
#4257=LINE('',#35497,#5326);
#4258=LINE('',#35501,#5327);
#4259=LINE('',#35504,#5328);
#4260=LINE('',#35505,#5329);
#4261=LINE('',#35511,#5330);
#4262=LINE('',#35513,#5331);
#4263=LINE('',#35515,#5332);
#4264=LINE('',#35516,#5333);
#4265=LINE('',#35520,#5334);
#4266=LINE('',#35523,#5335);
#4267=LINE('',#35524,#5336);
#4268=LINE('',#35530,#5337);
#4269=LINE('',#35532,#5338);
#4270=LINE('',#35534,#5339);
#4271=LINE('',#35535,#5340);
#4272=LINE('',#35539,#5341);
#4273=LINE('',#35542,#5342);
#4274=LINE('',#35543,#5343);
#4275=LINE('',#35549,#5344);
#4276=LINE('',#35551,#5345);
#4277=LINE('',#35553,#5346);
#4278=LINE('',#35554,#5347);
#4279=LINE('',#35558,#5348);
#4280=LINE('',#35561,#5349);
#4281=LINE('',#35562,#5350);
#4282=LINE('',#35568,#5351);
#4283=LINE('',#35570,#5352);
#4284=LINE('',#35572,#5353);
#4285=LINE('',#35573,#5354);
#4286=LINE('',#35577,#5355);
#4287=LINE('',#35580,#5356);
#4288=LINE('',#35581,#5357);
#4289=LINE('',#35587,#5358);
#4290=LINE('',#35589,#5359);
#4291=LINE('',#35591,#5360);
#4292=LINE('',#35592,#5361);
#4293=LINE('',#35596,#5362);
#4294=LINE('',#35599,#5363);
#4295=LINE('',#35600,#5364);
#4296=LINE('',#35606,#5365);
#4297=LINE('',#35608,#5366);
#4298=LINE('',#35610,#5367);
#4299=LINE('',#35611,#5368);
#4300=LINE('',#35615,#5369);
#4301=LINE('',#35618,#5370);
#4302=LINE('',#35619,#5371);
#4303=LINE('',#35625,#5372);
#4304=LINE('',#35627,#5373);
#4305=LINE('',#35629,#5374);
#4306=LINE('',#35630,#5375);
#4307=LINE('',#35634,#5376);
#4308=LINE('',#35637,#5377);
#4309=LINE('',#35638,#5378);
#4310=LINE('',#35644,#5379);
#4311=LINE('',#35646,#5380);
#4312=LINE('',#35648,#5381);
#4313=LINE('',#35649,#5382);
#4314=LINE('',#35653,#5383);
#4315=LINE('',#35656,#5384);
#4316=LINE('',#35657,#5385);
#4317=LINE('',#35663,#5386);
#4318=LINE('',#35665,#5387);
#4319=LINE('',#35667,#5388);
#4320=LINE('',#35668,#5389);
#4321=LINE('',#35672,#5390);
#4322=LINE('',#35675,#5391);
#4323=LINE('',#35676,#5392);
#4324=LINE('',#35682,#5393);
#4325=LINE('',#35684,#5394);
#4326=LINE('',#35686,#5395);
#4327=LINE('',#35687,#5396);
#4328=LINE('',#35691,#5397);
#4329=LINE('',#35694,#5398);
#4330=LINE('',#35695,#5399);
#4331=LINE('',#35701,#5400);
#4332=LINE('',#35703,#5401);
#4333=LINE('',#35705,#5402);
#4334=LINE('',#35706,#5403);
#4335=LINE('',#35710,#5404);
#4336=LINE('',#35713,#5405);
#4337=LINE('',#35714,#5406);
#4338=LINE('',#35720,#5407);
#4339=LINE('',#35722,#5408);
#4340=LINE('',#35724,#5409);
#4341=LINE('',#35725,#5410);
#4342=LINE('',#35729,#5411);
#4343=LINE('',#35732,#5412);
#4344=LINE('',#35733,#5413);
#4345=LINE('',#35739,#5414);
#4346=LINE('',#35741,#5415);
#4347=LINE('',#35743,#5416);
#4348=LINE('',#35744,#5417);
#4349=LINE('',#35749,#5418);
#4350=LINE('',#35753,#5419);
#4351=LINE('',#35754,#5420);
#4352=LINE('',#35762,#5421);
#4353=LINE('',#35764,#5422);
#4354=LINE('',#35766,#5423);
#4355=LINE('',#35767,#5424);
#4356=LINE('',#35771,#5425);
#4357=LINE('',#35774,#5426);
#4358=LINE('',#35775,#5427);
#4359=LINE('',#35781,#5428);
#4360=LINE('',#35783,#5429);
#4361=LINE('',#35785,#5430);
#4362=LINE('',#35786,#5431);
#4363=LINE('',#35790,#5432);
#4364=LINE('',#35793,#5433);
#4365=LINE('',#35794,#5434);
#4366=LINE('',#35800,#5435);
#4367=LINE('',#35802,#5436);
#4368=LINE('',#35804,#5437);
#4369=LINE('',#35805,#5438);
#4370=LINE('',#35809,#5439);
#4371=LINE('',#35812,#5440);
#4372=LINE('',#35813,#5441);
#4373=LINE('',#35819,#5442);
#4374=LINE('',#35821,#5443);
#4375=LINE('',#35823,#5444);
#4376=LINE('',#35824,#5445);
#4377=LINE('',#35828,#5446);
#4378=LINE('',#35831,#5447);
#4379=LINE('',#35832,#5448);
#4380=LINE('',#35838,#5449);
#4381=LINE('',#35840,#5450);
#4382=LINE('',#35842,#5451);
#4383=LINE('',#35843,#5452);
#4384=LINE('',#35847,#5453);
#4385=LINE('',#35850,#5454);
#4386=LINE('',#35851,#5455);
#4387=LINE('',#35857,#5456);
#4388=LINE('',#35859,#5457);
#4389=LINE('',#35861,#5458);
#4390=LINE('',#35862,#5459);
#4391=LINE('',#35866,#5460);
#4392=LINE('',#35869,#5461);
#4393=LINE('',#35870,#5462);
#4394=LINE('',#35876,#5463);
#4395=LINE('',#35878,#5464);
#4396=LINE('',#35880,#5465);
#4397=LINE('',#35881,#5466);
#4398=LINE('',#35885,#5467);
#4399=LINE('',#35888,#5468);
#4400=LINE('',#35889,#5469);
#4401=LINE('',#35895,#5470);
#4402=LINE('',#35897,#5471);
#4403=LINE('',#35899,#5472);
#4404=LINE('',#35900,#5473);
#4405=LINE('',#35904,#5474);
#4406=LINE('',#35907,#5475);
#4407=LINE('',#35908,#5476);
#4408=LINE('',#35914,#5477);
#4409=LINE('',#35916,#5478);
#4410=LINE('',#35918,#5479);
#4411=LINE('',#35919,#5480);
#4412=LINE('',#35923,#5481);
#4413=LINE('',#35926,#5482);
#4414=LINE('',#35927,#5483);
#4415=LINE('',#35933,#5484);
#4416=LINE('',#35935,#5485);
#4417=LINE('',#35937,#5486);
#4418=LINE('',#35938,#5487);
#4419=LINE('',#35942,#5488);
#4420=LINE('',#35945,#5489);
#4421=LINE('',#35946,#5490);
#4422=LINE('',#35952,#5491);
#4423=LINE('',#35954,#5492);
#4424=LINE('',#35956,#5493);
#4425=LINE('',#35957,#5494);
#4426=LINE('',#35961,#5495);
#4427=LINE('',#35964,#5496);
#4428=LINE('',#35965,#5497);
#4429=LINE('',#35971,#5498);
#4430=LINE('',#35973,#5499);
#4431=LINE('',#35975,#5500);
#4432=LINE('',#35976,#5501);
#4433=LINE('',#35980,#5502);
#4434=LINE('',#35983,#5503);
#4435=LINE('',#35984,#5504);
#4436=LINE('',#35990,#5505);
#4437=LINE('',#35992,#5506);
#4438=LINE('',#35994,#5507);
#4439=LINE('',#35995,#5508);
#4440=LINE('',#35999,#5509);
#4441=LINE('',#36002,#5510);
#4442=LINE('',#36003,#5511);
#4443=LINE('',#36009,#5512);
#4444=LINE('',#36011,#5513);
#4445=LINE('',#36013,#5514);
#4446=LINE('',#36014,#5515);
#4447=LINE('',#36018,#5516);
#4448=LINE('',#36021,#5517);
#4449=LINE('',#36022,#5518);
#4450=LINE('',#36028,#5519);
#4451=LINE('',#36030,#5520);
#4452=LINE('',#36032,#5521);
#4453=LINE('',#36033,#5522);
#4454=LINE('',#36037,#5523);
#4455=LINE('',#36040,#5524);
#4456=LINE('',#36041,#5525);
#4457=LINE('',#36047,#5526);
#4458=LINE('',#36049,#5527);
#4459=LINE('',#36051,#5528);
#4460=LINE('',#36052,#5529);
#4461=LINE('',#36056,#5530);
#4462=LINE('',#36059,#5531);
#4463=LINE('',#36060,#5532);
#4464=LINE('',#36066,#5533);
#4465=LINE('',#36068,#5534);
#4466=LINE('',#36070,#5535);
#4467=LINE('',#36071,#5536);
#4468=LINE('',#36075,#5537);
#4469=LINE('',#36078,#5538);
#4470=LINE('',#36079,#5539);
#4471=LINE('',#36085,#5540);
#4472=LINE('',#36087,#5541);
#4473=LINE('',#36089,#5542);
#4474=LINE('',#36090,#5543);
#4475=LINE('',#36094,#5544);
#4476=LINE('',#36097,#5545);
#4477=LINE('',#36098,#5546);
#4478=LINE('',#36104,#5547);
#4479=LINE('',#36106,#5548);
#4480=LINE('',#36108,#5549);
#4481=LINE('',#36109,#5550);
#4482=LINE('',#36112,#5551);
#4483=LINE('',#36114,#5552);
#4484=LINE('',#36115,#5553);
#4485=LINE('',#36118,#5554);
#4486=LINE('',#36120,#5555);
#4487=LINE('',#36121,#5556);
#4488=LINE('',#36124,#5557);
#4489=LINE('',#36126,#5558);
#4490=LINE('',#36127,#5559);
#4491=LINE('',#36130,#5560);
#4492=LINE('',#36132,#5561);
#4493=LINE('',#36133,#5562);
#4494=LINE('',#36135,#5563);
#4495=LINE('',#36136,#5564);
#4496=LINE('',#36142,#5565);
#4497=LINE('',#36151,#5566);
#4498=LINE('',#36152,#5567);
#4499=LINE('',#36156,#5568);
#4500=LINE('',#36162,#5569);
#4501=LINE('',#36195,#5570);
#4502=LINE('',#36285,#5571);
#4503=LINE('',#36369,#5572);
#4504=LINE('',#36459,#5573);
#4505=LINE('',#36549,#5574);
#4506=LINE('',#36639,#5575);
#4507=LINE('',#36723,#5576);
#4508=LINE('',#36734,#5577);
#4509=LINE('',#36771,#5578);
#4510=LINE('',#36808,#5579);
#4511=LINE('',#36846,#5580);
#4512=LINE('',#36884,#5581);
#4513=LINE('',#36921,#5582);
#4514=LINE('',#36958,#5583);
#4515=LINE('',#36960,#5584);
#4516=LINE('',#36961,#5585);
#4517=LINE('',#36965,#5586);
#4518=LINE('',#36966,#5587);
#4519=LINE('',#36967,#5588);
#4520=LINE('',#36971,#5589);
#4521=LINE('',#36973,#5590);
#4522=LINE('',#36974,#5591);
#4523=LINE('',#36978,#5592);
#4524=LINE('',#36979,#5593);
#4525=LINE('',#36980,#5594);
#4526=LINE('',#36982,#5595);
#4527=LINE('',#36983,#5596);
#4528=LINE('',#36987,#5597);
#4529=LINE('',#36989,#5598);
#4530=LINE('',#36990,#5599);
#4531=LINE('',#36994,#5600);
#4532=LINE('',#36995,#5601);
#4533=LINE('',#36996,#5602);
#4534=LINE('',#37000,#5603);
#4535=LINE('',#37002,#5604);
#4536=LINE('',#37003,#5605);
#4537=LINE('',#37007,#5606);
#4538=LINE('',#37008,#5607);
#4539=LINE('',#37009,#5608);
#4540=LINE('',#37011,#5609);
#4541=LINE('',#37012,#5610);
#4542=LINE('',#37016,#5611);
#4543=LINE('',#37018,#5612);
#4544=LINE('',#37019,#5613);
#4545=LINE('',#37023,#5614);
#4546=LINE('',#37024,#5615);
#4547=LINE('',#37025,#5616);
#4548=LINE('',#37029,#5617);
#4549=LINE('',#37031,#5618);
#4550=LINE('',#37032,#5619);
#4551=LINE('',#37036,#5620);
#4552=LINE('',#37037,#5621);
#4553=LINE('',#37038,#5622);
#4554=LINE('',#37040,#5623);
#4555=LINE('',#37041,#5624);
#4556=LINE('',#37043,#5625);
#4557=LINE('',#37044,#5626);
#4558=LINE('',#37046,#5627);
#4559=LINE('',#37047,#5628);
#4560=LINE('',#37049,#5629);
#4561=LINE('',#37050,#5630);
#4562=LINE('',#37052,#5631);
#4563=LINE('',#37054,#5632);
#4564=LINE('',#37056,#5633);
#4565=LINE('',#37060,#5634);
#4566=LINE('',#37062,#5635);
#4567=LINE('',#37064,#5636);
#4568=LINE('',#37066,#5637);
#4569=LINE('',#37068,#5638);
#4570=LINE('',#37069,#5639);
#4571=LINE('',#37072,#5640);
#4572=LINE('',#37074,#5641);
#4573=LINE('',#37075,#5642);
#4574=LINE('',#37078,#5643);
#4575=LINE('',#37079,#5644);
#4576=LINE('',#37082,#5645);
#4577=LINE('',#37084,#5646);
#4578=LINE('',#37085,#5647);
#4579=LINE('',#37088,#5648);
#4580=LINE('',#37089,#5649);
#4581=LINE('',#37091,#5650);
#4582=LINE('',#37093,#5651);
#4583=LINE('',#37096,#5652);
#4584=LINE('',#37098,#5653);
#4585=LINE('',#37099,#5654);
#4586=LINE('',#37102,#5655);
#4587=LINE('',#37103,#5656);
#4588=LINE('',#37106,#5657);
#4589=LINE('',#37107,#5658);
#4590=LINE('',#38411,#5659);
#4591=LINE('',#38412,#5660);
#4592=LINE('',#38415,#5661);
#4593=LINE('',#38416,#5662);
#4594=LINE('',#38418,#5663);
#4595=LINE('',#38421,#5664);
#4596=LINE('',#38423,#5665);
#4597=LINE('',#38425,#5666);
#4598=LINE('',#38435,#5667);
#4599=LINE('',#38440,#5668);
#4600=LINE('',#38443,#5669);
#4601=VECTOR('',#16783,14.75);
#4602=VECTOR('',#16788,15.);
#4603=VECTOR('',#16801,7.4);
#4604=VECTOR('',#16806,10.);
#4605=VECTOR('',#16809,10.);
#4606=VECTOR('',#16812,10.);
#4607=VECTOR('',#16819,7.15);
#4608=VECTOR('',#16824,14.75);
#4609=VECTOR('',#16833,15.);
#4610=VECTOR('',#16842,7.4);
#4611=VECTOR('',#16847,10.);
#4612=VECTOR('',#16850,10.);
#4613=VECTOR('',#16853,10.);
#4614=VECTOR('',#16860,7.15);
#4615=VECTOR('',#16863,9.3);
#4616=VECTOR('',#16868,9.05);
#4617=VECTOR('',#16875,6.3);
#4618=VECTOR('',#16880,10.);
#4619=VECTOR('',#16883,10.);
#4620=VECTOR('',#16886,10.);
#4621=VECTOR('',#16889,10.);
#4622=VECTOR('',#16902,6.05);
#4623=VECTOR('',#16907,6.3);
#4624=VECTOR('',#16912,6.05);
#4625=VECTOR('',#16917,6.3);
#4626=VECTOR('',#16922,6.05);
#4627=VECTOR('',#16927,6.3);
#4628=VECTOR('',#16932,6.05);
#4629=VECTOR('',#16941,10.);
#4630=VECTOR('',#16944,10.);
#4631=VECTOR('',#16947,10.);
#4632=VECTOR('',#16948,10.);
#4633=VECTOR('',#16949,10.);
#4634=VECTOR('',#16950,10.);
#4635=VECTOR('',#16951,10.);
#4636=VECTOR('',#16952,10.);
#4637=VECTOR('',#16955,10.);
#4638=VECTOR('',#16958,10.);
#4639=VECTOR('',#16961,10.);
#4640=VECTOR('',#16962,10.);
#4641=VECTOR('',#16963,10.);
#4642=VECTOR('',#16964,10.);
#4643=VECTOR('',#16965,10.);
#4644=VECTOR('',#16966,10.);
#4645=VECTOR('',#16967,10.);
#4646=VECTOR('',#16968,10.);
#4647=VECTOR('',#16973,10.);
#4648=VECTOR('',#16980,10.);
#4649=VECTOR('',#16983,10.);
#4650=VECTOR('',#16986,10.);
#4651=VECTOR('',#16989,10.);
#4652=VECTOR('',#17002,10.);
#4653=VECTOR('',#17005,10.);
#4654=VECTOR('',#17008,10.);
#4655=VECTOR('',#17009,10.);
#4656=VECTOR('',#17010,10.);
#4657=VECTOR('',#17011,10.);
#4658=VECTOR('',#17012,10.);
#4659=VECTOR('',#17015,10.);
#4660=VECTOR('',#17018,10.);
#4661=VECTOR('',#17021,10.);
#4662=VECTOR('',#17022,10.);
#4663=VECTOR('',#17023,10.);
#4664=VECTOR('',#17024,10.);
#4665=VECTOR('',#17025,10.);
#4666=VECTOR('',#17026,10.);
#4667=VECTOR('',#17027,10.);
#4668=VECTOR('',#17028,10.);
#4669=VECTOR('',#17033,10.);
#4670=VECTOR('',#17042,10.);
#4671=VECTOR('',#17045,10.);
#4672=VECTOR('',#17048,10.);
#4673=VECTOR('',#17059,7.4);
#4674=VECTOR('',#17064,10.);
#4675=VECTOR('',#17067,10.);
#4676=VECTOR('',#17070,10.);
#4677=VECTOR('',#17073,10.);
#4678=VECTOR('',#17080,7.4);
#4679=VECTOR('',#17087,10.);
#4680=VECTOR('',#17096,10.);
#4681=VECTOR('',#17109,10.);
#4682=VECTOR('',#17112,10.);
#4683=VECTOR('',#17115,10.);
#4684=VECTOR('',#17118,10.);
#4685=VECTOR('',#17121,10.);
#4686=VECTOR('',#17130,10.);
#4687=VECTOR('',#17139,10.);
#4688=VECTOR('',#17142,10.);
#4689=VECTOR('',#17145,10.);
#4690=VECTOR('',#17156,10.);
#4691=VECTOR('',#17175,50.8);
#4692=VECTOR('',#17178,10.);
#4693=VECTOR('',#17191,10.);
#4694=VECTOR('',#17206,10.);
#4695=VECTOR('',#17209,10.);
#4696=VECTOR('',#17214,10.);
#4697=VECTOR('',#17227,10.);
#4698=VECTOR('',#17232,10.);
#4699=VECTOR('',#17245,10.);
#4700=VECTOR('',#17304,50.);
#4701=VECTOR('',#17317,9.05);
#4702=VECTOR('',#17330,23.525);
#4703=VECTOR('',#17339,27.505);
#4704=VECTOR('',#17348,26.);
#4705=VECTOR('',#17369,13.25);
#4706=VECTOR('',#17380,13.);
#4707=VECTOR('',#17387,19.25);
#4708=VECTOR('',#17394,10.);
#4709=VECTOR('',#17397,10.);
#4710=VECTOR('',#17400,10.);
#4711=VECTOR('',#17403,10.);
#4712=VECTOR('',#17406,19.);
#4713=VECTOR('',#17411,10.);
#4714=VECTOR('',#17416,10.);
#4715=VECTOR('',#17417,10.);
#4716=VECTOR('',#17418,10.);
#4717=VECTOR('',#17421,10.);
#4718=VECTOR('',#17424,10.);
#4719=VECTOR('',#17427,10.);
#4720=VECTOR('',#17428,10.);
#4721=VECTOR('',#17431,10.);
#4722=VECTOR('',#17432,10.);
#4723=VECTOR('',#17435,10.);
#4724=VECTOR('',#17438,10.);
#4725=VECTOR('',#17443,6.05);
#4726=VECTOR('',#17448,10.);
#4727=VECTOR('',#17451,10.);
#4728=VECTOR('',#17452,10.);
#4729=VECTOR('',#17453,10.);
#4730=VECTOR('',#17456,10.);
#4731=VECTOR('',#17459,10.);
#4732=VECTOR('',#17462,10.);
#4733=VECTOR('',#17463,10.);
#4734=VECTOR('',#17466,10.);
#4735=VECTOR('',#17467,10.);
#4736=VECTOR('',#17472,10.);
#4737=VECTOR('',#17477,6.05);
#4738=VECTOR('',#17482,10.);
#4739=VECTOR('',#17485,10.);
#4740=VECTOR('',#17488,10.);
#4741=VECTOR('',#17489,10.);
#4742=VECTOR('',#17492,10.);
#4743=VECTOR('',#17497,10.);
#4744=VECTOR('',#17498,10.);
#4745=VECTOR('',#17499,10.);
#4746=VECTOR('',#17502,6.05);
#4747=VECTOR('',#17507,10.);
#4748=VECTOR('',#17510,10.);
#4749=VECTOR('',#17511,10.);
#4750=VECTOR('',#17512,10.);
#4751=VECTOR('',#17515,10.);
#4752=VECTOR('',#17518,10.);
#4753=VECTOR('',#17521,10.);
#4754=VECTOR('',#17522,10.);
#4755=VECTOR('',#17525,10.);
#4756=VECTOR('',#17526,10.);
#4757=VECTOR('',#17531,10.);
#4758=VECTOR('',#17536,6.05);
#4759=VECTOR('',#17539,10.);
#4760=VECTOR('',#17544,10.);
#4761=VECTOR('',#17549,10.);
#4762=VECTOR('',#17552,2.);
#4763=VECTOR('',#17553,10.);
#4764=VECTOR('',#17556,10.);
#4765=VECTOR('',#17575,10.);
#4766=VECTOR('',#17582,10.);
#4767=VECTOR('',#17583,10.);
#4768=VECTOR('',#17584,10.);
#4769=VECTOR('',#17591,10.);
#4770=VECTOR('',#17594,10.);
#4771=VECTOR('',#17595,10.);
#4772=VECTOR('',#17600,5.30000000000001);
#4773=VECTOR('',#17605,10.);
#4774=VECTOR('',#17606,10.);
#4775=VECTOR('',#17607,10.);
#4776=VECTOR('',#17608,10.);
#4777=VECTOR('',#17619,5.05000000000001);
#4778=VECTOR('',#17624,5.29999999999999);
#4779=VECTOR('',#17629,5.04999999999999);
#4780=VECTOR('',#17634,5.29999999999999);
#4781=VECTOR('',#17639,5.04999999999999);
#4782=VECTOR('',#17644,5.30000000000001);
#4783=VECTOR('',#17649,5.05000000000001);
#4784=VECTOR('',#17654,9.75);
#4785=VECTOR('',#17659,9.49999999999999);
#4786=VECTOR('',#17668,6.);
#4787=VECTOR('',#17673,10.);
#4788=VECTOR('',#17674,10.);
#4789=VECTOR('',#17687,10.);
#4790=VECTOR('',#17690,10.);
#4791=VECTOR('',#17691,10.);
#4792=VECTOR('',#17696,10.);
#4793=VECTOR('',#17705,10.);
#4794=VECTOR('',#17712,10.);
#4795=VECTOR('',#17713,10.);
#4796=VECTOR('',#17714,10.);
#4797=VECTOR('',#17735,10.);
#4798=VECTOR('',#17736,10.);
#4799=VECTOR('',#17739,10.);
#4800=VECTOR('',#17742,10.);
#4801=VECTOR('',#17753,10.);
#4802=VECTOR('',#17754,10.);
#4803=VECTOR('',#17757,10.);
#4804=VECTOR('',#17760,10.);
#4805=VECTOR('',#17767,10.);
#4806=VECTOR('',#17772,10.);
#4807=VECTOR('',#17795,43.05);
#4808=VECTOR('',#17808,10.);
#4809=VECTOR('',#17843,10.);
#4810=VECTOR('',#17846,10.);
#4811=VECTOR('',#17849,10.);
#4812=VECTOR('',#17888,10.);
#4813=VECTOR('',#17897,10.);
#4814=VECTOR('',#17900,10.);
#4815=VECTOR('',#17901,10.);
#4816=VECTOR('',#17904,10.);
#4817=VECTOR('',#17907,10.);
#4818=VECTOR('',#17920,10.);
#4819=VECTOR('',#17947,10.);
#4820=VECTOR('',#17948,10.);
#4821=VECTOR('',#17953,10.);
#4822=VECTOR('',#17954,10.);
#4823=VECTOR('',#17957,10.);
#4824=VECTOR('',#17960,10.);
#4825=VECTOR('',#17963,10.);
#4826=VECTOR('',#17966,10.);
#4827=VECTOR('',#17979,10.);
#4828=VECTOR('',#17982,2.);
#4829=VECTOR('',#17987,10.);
#4830=VECTOR('',#18032,10.);
#4831=VECTOR('',#18037,10.);
#4832=VECTOR('',#18050,10.);
#4833=VECTOR('',#18053,6.5);
#4834=VECTOR('',#18058,6.5);
#4835=VECTOR('',#18061,6.5);
#4836=VECTOR('',#18064,6.5);
#4837=VECTOR('',#18093,16.6);
#4838=VECTOR('',#18102,16.505);
#4839=VECTOR('',#18113,10.);
#4840=VECTOR('',#18116,10.);
#4841=VECTOR('',#18119,10.);
#4842=VECTOR('',#18120,10.);
#4843=VECTOR('',#18121,10.);
#4844=VECTOR('',#18128,10.);
#4845=VECTOR('',#18139,10.);
#4846=VECTOR('',#18142,10.);
#4847=VECTOR('',#18151,10.);
#4848=VECTOR('',#18152,10.);
#4849=VECTOR('',#18161,10.);
#4850=VECTOR('',#18166,10.);
#4851=VECTOR('',#18169,20.);
#4852=VECTOR('',#18180,41.4267766952966);
#4853=VECTOR('',#18199,10.);
#4854=VECTOR('',#18202,10.);
#4855=VECTOR('',#18203,10.);
#4856=VECTOR('',#18208,42.);
#4857=VECTOR('',#18211,10.);
#4858=VECTOR('',#18214,10.);
#4859=VECTOR('',#18219,10.);
#4860=VECTOR('',#18220,10.);
#4861=VECTOR('',#18223,10.);
#4862=VECTOR('',#18226,10.);
#4863=VECTOR('',#18227,10.);
#4864=VECTOR('',#18228,10.);
#4865=VECTOR('',#18231,10.);
#4866=VECTOR('',#18232,10.);
#4867=VECTOR('',#18241,10.);
#4868=VECTOR('',#18244,10.);
#4869=VECTOR('',#18247,10.);
#4870=VECTOR('',#18248,10.);
#4871=VECTOR('',#18251,10.);
#4872=VECTOR('',#18252,10.);
#4873=VECTOR('',#18255,10.);
#4874=VECTOR('',#18276,5.);
#4875=VECTOR('',#18281,8.51);
#4876=VECTOR('',#18288,5.);
#4877=VECTOR('',#18293,8.51);
#4878=VECTOR('',#18300,5.);
#4879=VECTOR('',#18305,8.51);
#4880=VECTOR('',#18312,5.);
#4881=VECTOR('',#18317,8.51);
#4882=VECTOR('',#18324,5.);
#4883=VECTOR('',#18329,8.51);
#4884=VECTOR('',#18336,5.);
#4885=VECTOR('',#18341,8.51);
#4886=VECTOR('',#18348,5.);
#4887=VECTOR('',#18353,8.51);
#4888=VECTOR('',#18360,42.5);
#4889=VECTOR('',#18367,10.);
#4890=VECTOR('',#18370,10.);
#4891=VECTOR('',#18373,10.);
#4892=VECTOR('',#18374,10.);
#4893=VECTOR('',#18375,10.);
#4894=VECTOR('',#18382,10.);
#4895=VECTOR('',#18387,10.);
#4896=VECTOR('',#18390,10.);
#4897=VECTOR('',#18393,10.);
#4898=VECTOR('',#18394,10.);
#4899=VECTOR('',#18395,10.);
#4900=VECTOR('',#18402,10.);
#4901=VECTOR('',#18407,10.);
#4902=VECTOR('',#18410,10.);
#4903=VECTOR('',#18413,10.);
#4904=VECTOR('',#18414,10.);
#4905=VECTOR('',#18415,10.);
#4906=VECTOR('',#18422,10.);
#4907=VECTOR('',#18427,10.);
#4908=VECTOR('',#18430,10.);
#4909=VECTOR('',#18433,10.);
#4910=VECTOR('',#18434,10.);
#4911=VECTOR('',#18435,10.);
#4912=VECTOR('',#18442,10.);
#4913=VECTOR('',#18471,15.5);
#4914=VECTOR('',#18482,43.);
#4915=VECTOR('',#18489,10.);
#4916=VECTOR('',#18490,10.);
#4917=VECTOR('',#18493,10.);
#4918=VECTOR('',#18494,10.);
#4919=VECTOR('',#18503,10.);
#4920=VECTOR('',#18504,10.);
#4921=VECTOR('',#18505,10.);
#4922=VECTOR('',#18506,10.);
#4923=VECTOR('',#18509,10.);
#4924=VECTOR('',#18510,10.);
#4925=VECTOR('',#18513,10.);
#4926=VECTOR('',#18514,10.);
#4927=VECTOR('',#18515,10.);
#4928=VECTOR('',#18518,10.);
#4929=VECTOR('',#18519,10.);
#4930=VECTOR('',#18522,10.);
#4931=VECTOR('',#18523,10.);
#4932=VECTOR('',#18532,10.);
#4933=VECTOR('',#18533,10.);
#4934=VECTOR('',#18534,10.);
#4935=VECTOR('',#18535,10.);
#4936=VECTOR('',#18538,10.);
#4937=VECTOR('',#18539,10.);
#4938=VECTOR('',#18542,10.);
#4939=VECTOR('',#18543,10.);
#4940=VECTOR('',#18544,10.);
#4941=VECTOR('',#18547,10.);
#4942=VECTOR('',#18548,10.);
#4943=VECTOR('',#18551,10.);
#4944=VECTOR('',#18552,10.);
#4945=VECTOR('',#18561,10.);
#4946=VECTOR('',#18562,10.);
#4947=VECTOR('',#18563,10.);
#4948=VECTOR('',#18564,10.);
#4949=VECTOR('',#18567,10.);
#4950=VECTOR('',#18568,10.);
#4951=VECTOR('',#18571,10.);
#4952=VECTOR('',#18572,10.);
#4953=VECTOR('',#18573,10.);
#4954=VECTOR('',#18576,10.);
#4955=VECTOR('',#18577,10.);
#4956=VECTOR('',#18580,10.);
#4957=VECTOR('',#18581,10.);
#4958=VECTOR('',#18590,10.);
#4959=VECTOR('',#18591,10.);
#4960=VECTOR('',#18592,10.);
#4961=VECTOR('',#18593,10.);
#4962=VECTOR('',#18596,10.);
#4963=VECTOR('',#18597,10.);
#4964=VECTOR('',#18600,10.);
#4965=VECTOR('',#18601,10.);
#4966=VECTOR('',#18602,10.);
#4967=VECTOR('',#18605,10.);
#4968=VECTOR('',#18606,10.);
#4969=VECTOR('',#18609,10.);
#4970=VECTOR('',#18610,10.);
#4971=VECTOR('',#18611,10.);
#4972=VECTOR('',#18612,10.);
#4973=VECTOR('',#18615,10.);
#4974=VECTOR('',#18616,10.);
#4975=VECTOR('',#18625,10.);
#4976=VECTOR('',#18626,10.);
#4977=VECTOR('',#18627,10.);
#4978=VECTOR('',#18628,10.);
#4979=VECTOR('',#18639,11.1);
#4980=VECTOR('',#18642,10.);
#4981=VECTOR('',#18645,10.);
#4982=VECTOR('',#18648,10.);
#4983=VECTOR('',#18651,10.);
#4984=VECTOR('',#18654,10.);
#4985=VECTOR('',#18657,10.);
#4986=VECTOR('',#18660,10.);
#4987=VECTOR('',#18671,10.);
#4988=VECTOR('',#18674,10.);
#4989=VECTOR('',#18677,10.);
#4990=VECTOR('',#18680,10.);
#4991=VECTOR('',#18683,10.);
#4992=VECTOR('',#18686,10.);
#4993=VECTOR('',#18689,10.);
#4994=VECTOR('',#18692,10.);
#4995=VECTOR('',#18695,10.);
#4996=VECTOR('',#18700,10.);
#4997=VECTOR('',#18703,10.);
#4998=VECTOR('',#18710,10.);
#4999=VECTOR('',#18711,10.);
#5000=VECTOR('',#18712,10.);
#5001=VECTOR('',#18713,10.);
#5002=VECTOR('',#18716,10.);
#5003=VECTOR('',#18717,10.);
#5004=VECTOR('',#18720,10.);
#5005=VECTOR('',#18721,10.);
#5006=VECTOR('',#18722,10.);
#5007=VECTOR('',#18725,10.);
#5008=VECTOR('',#18728,10.);
#5009=VECTOR('',#18735,10.);
#5010=VECTOR('',#18736,10.);
#5011=VECTOR('',#18737,10.);
#5012=VECTOR('',#18738,10.);
#5013=VECTOR('',#18741,10.);
#5014=VECTOR('',#18742,10.);
#5015=VECTOR('',#18745,10.);
#5016=VECTOR('',#18746,10.);
#5017=VECTOR('',#18747,10.);
#5018=VECTOR('',#18750,10.);
#5019=VECTOR('',#18751,10.);
#5020=VECTOR('',#18752,10.);
#5021=VECTOR('',#18753,10.);
#5022=VECTOR('',#18756,10.);
#5023=VECTOR('',#18757,10.);
#5024=VECTOR('',#18758,10.);
#5025=VECTOR('',#18761,10.);
#5026=VECTOR('',#18762,10.);
#5027=VECTOR('',#18763,10.);
#5028=VECTOR('',#18764,10.);
#5029=VECTOR('',#18767,10.);
#5030=VECTOR('',#18768,10.);
#5031=VECTOR('',#18769,10.);
#5032=VECTOR('',#18772,10.);
#5033=VECTOR('',#18773,10.);
#5034=VECTOR('',#18774,10.);
#5035=VECTOR('',#18775,10.);
#5036=VECTOR('',#18778,10.);
#5037=VECTOR('',#18779,10.);
#5038=VECTOR('',#18780,10.);
#5039=VECTOR('',#18783,10.);
#5040=VECTOR('',#18784,10.);
#5041=VECTOR('',#18785,10.);
#5042=VECTOR('',#18786,10.);
#5043=VECTOR('',#18789,10.);
#5044=VECTOR('',#18790,10.);
#5045=VECTOR('',#18791,10.);
#5046=VECTOR('',#18794,10.);
#5047=VECTOR('',#18795,10.);
#5048=VECTOR('',#18796,10.);
#5049=VECTOR('',#18797,10.);
#5050=VECTOR('',#18800,10.);
#5051=VECTOR('',#18801,10.);
#5052=VECTOR('',#18802,10.);
#5053=VECTOR('',#18805,10.);
#5054=VECTOR('',#18806,10.);
#5055=VECTOR('',#18811,10.);
#5056=VECTOR('',#18812,10.);
#5057=VECTOR('',#18817,10.);
#5058=VECTOR('',#18818,10.);
#5059=VECTOR('',#18821,10.);
#5060=VECTOR('',#18824,10.);
#5061=VECTOR('',#18825,10.);
#5062=VECTOR('',#18830,10.);
#5063=VECTOR('',#18831,10.);
#5064=VECTOR('',#18836,10.);
#5065=VECTOR('',#18837,10.);
#5066=VECTOR('',#18842,10.);
#5067=VECTOR('',#18843,10.);
#5068=VECTOR('',#18848,10.);
#5069=VECTOR('',#18851,10.);
#5070=VECTOR('',#18858,10.);
#5071=VECTOR('',#18859,10.);
#5072=VECTOR('',#18862,10.);
#5073=VECTOR('',#18865,10.);
#5074=VECTOR('',#18868,10.);
#5075=VECTOR('',#18871,10.);
#5076=VECTOR('',#18878,10.);
#5077=VECTOR('',#18879,10.);
#5078=VECTOR('',#18882,10.);
#5079=VECTOR('',#18885,10.);
#5080=VECTOR('',#18888,10.);
#5081=VECTOR('',#18891,10.);
#5082=VECTOR('',#18898,10.);
#5083=VECTOR('',#18899,10.);
#5084=VECTOR('',#18902,10.);
#5085=VECTOR('',#18905,10.);
#5086=VECTOR('',#18908,10.);
#5087=VECTOR('',#18911,10.);
#5088=VECTOR('',#18918,10.);
#5089=VECTOR('',#18919,10.);
#5090=VECTOR('',#18922,10.);
#5091=VECTOR('',#18925,10.);
#5092=VECTOR('',#18928,10.);
#5093=VECTOR('',#18931,10.);
#5094=VECTOR('',#18938,10.);
#5095=VECTOR('',#18939,10.);
#5096=VECTOR('',#18942,10.);
#5097=VECTOR('',#18949,10.);
#5098=VECTOR('',#18950,10.);
#5099=VECTOR('',#18951,10.);
#5100=VECTOR('',#18952,10.);
#5101=VECTOR('',#18955,10.);
#5102=VECTOR('',#18956,10.);
#5103=VECTOR('',#18957,10.);
#5104=VECTOR('',#18960,10.);
#5105=VECTOR('',#18963,10.);
#5106=VECTOR('',#18970,10.);
#5107=VECTOR('',#18971,10.);
#5108=VECTOR('',#18974,10.);
#5109=VECTOR('',#18983,3.6);
#5110=VECTOR('',#18988,3.35);
#5111=VECTOR('',#18993,10.);
#5112=VECTOR('',#19014,10.);
#5113=VECTOR('',#19021,10.);
#5114=VECTOR('',#19022,10.);
#5115=VECTOR('',#19023,10.);
#5116=VECTOR('',#19026,10.);
#5117=VECTOR('',#19027,10.);
#5118=VECTOR('',#19028,10.);
#5119=VECTOR('',#19031,10.);
#5120=VECTOR('',#19032,10.);
#5121=VECTOR('',#19033,10.);
#5122=VECTOR('',#19038,10.);
#5123=VECTOR('',#19075,15.);
#5124=VECTOR('',#19084,14.);
#5125=VECTOR('',#19093,12.5);
#5126=VECTOR('',#19098,12.25);
#5127=VECTOR('',#19105,10.);
#5128=VECTOR('',#19106,10.);
#5129=VECTOR('',#19107,10.);
#5130=VECTOR('',#19108,10.);
#5131=VECTOR('',#19109,10.);
#5132=VECTOR('',#19110,10.);
#5133=VECTOR('',#19113,10.);
#5134=VECTOR('',#19114,10.);
#5135=VECTOR('',#19115,10.);
#5136=VECTOR('',#19118,10.);
#5137=VECTOR('',#19119,10.);
#5138=VECTOR('',#19120,10.);
#5139=VECTOR('',#19121,10.);
#5140=VECTOR('',#19124,10.);
#5141=VECTOR('',#19125,10.);
#5142=VECTOR('',#19126,10.);
#5143=VECTOR('',#19127,10.);
#5144=VECTOR('',#19130,10.);
#5145=VECTOR('',#19131,10.);
#5146=VECTOR('',#19132,10.);
#5147=VECTOR('',#19133,10.);
#5148=VECTOR('',#19134,10.);
#5149=VECTOR('',#19137,10.);
#5150=VECTOR('',#19138,10.);
#5151=VECTOR('',#19139,10.);
#5152=VECTOR('',#19142,10.);
#5153=VECTOR('',#19143,10.);
#5154=VECTOR('',#19144,10.);
#5155=VECTOR('',#19145,10.);
#5156=VECTOR('',#19148,10.);
#5157=VECTOR('',#19149,10.);
#5158=VECTOR('',#19150,10.);
#5159=VECTOR('',#19153,10.);
#5160=VECTOR('',#19154,10.);
#5161=VECTOR('',#19157,10.);
#5162=VECTOR('',#19158,10.);
#5163=VECTOR('',#19159,10.);
#5164=VECTOR('',#19160,10.);
#5165=VECTOR('',#19163,10.);
#5166=VECTOR('',#19164,10.);
#5167=VECTOR('',#19165,10.);
#5168=VECTOR('',#19168,10.);
#5169=VECTOR('',#19169,10.);
#5170=VECTOR('',#19172,10.);
#5171=VECTOR('',#19173,10.);
#5172=VECTOR('',#19174,10.);
#5173=VECTOR('',#19177,10.);
#5174=VECTOR('',#19180,10.);
#5175=VECTOR('',#19193,19.15);
#5176=VECTOR('',#19202,23.9);
#5177=VECTOR('',#19213,27.3);
#5178=VECTOR('',#19218,27.5);
#5179=VECTOR('',#19223,27.3);
#5180=VECTOR('',#19230,23.9);
#5181=VECTOR('',#19241,19.15);
#5182=VECTOR('',#19248,15.2);
#5183=VECTOR('',#19253,15.);
#5184=VECTOR('',#19258,15.2);
#5185=VECTOR('',#19269,12.5);
#5186=VECTOR('',#19284,15.6);
#5187=VECTOR('',#19289,13.5);
#5188=VECTOR('',#19300,16.5);
#5189=VECTOR('',#19307,13.5);
#5190=VECTOR('',#19314,15.6);
#5191=VECTOR('',#19327,20.64);
#5192=VECTOR('',#19336,20.5);
#5193=VECTOR('',#19345,16.9764870412073);
#5194=VECTOR('',#19356,17.75);
#5195=VECTOR('',#19361,15.);
#5196=VECTOR('',#19368,23.52);
#5197=VECTOR('',#19375,16.5);
#5198=VECTOR('',#19382,4.25);
#5199=VECTOR('',#19389,4.);
#5200=VECTOR('',#19398,1.);
#5201=VECTOR('',#19409,4.);
#5202=VECTOR('',#19422,8.25);
#5203=VECTOR('',#19427,8.5);
#5204=VECTOR('',#19430,8.25);
#5205=VECTOR('',#19439,5.);
#5206=VECTOR('',#19450,10.75);
#5207=VECTOR('',#19455,11.);
#5208=VECTOR('',#19464,9.);
#5209=VECTOR('',#19483,2.);
#5210=VECTOR('',#19494,40.9);
#5211=VECTOR('',#19531,41.);
#5212=VECTOR('',#19538,10.);
#5213=VECTOR('',#19539,10.);
#5214=VECTOR('',#19544,10.);
#5215=VECTOR('',#19549,10.);
#5216=VECTOR('',#19554,10.);
#5217=VECTOR('',#19559,10.);
#5218=VECTOR('',#19564,10.);
#5219=VECTOR('',#19569,10.);
#5220=VECTOR('',#19574,10.);
#5221=VECTOR('',#19579,10.);
#5222=VECTOR('',#19584,10.);
#5223=VECTOR('',#19589,10.);
#5224=VECTOR('',#19594,10.);
#5225=VECTOR('',#19599,10.);
#5226=VECTOR('',#19610,40.75);
#5227=VECTOR('',#19615,6.);
#5228=VECTOR('',#19620,6.);
#5229=VECTOR('',#19623,6.);
#5230=VECTOR('',#19626,6.);
#5231=VECTOR('',#19629,6.);
#5232=VECTOR('',#19632,6.);
#5233=VECTOR('',#19635,6.);
#5234=VECTOR('',#19638,6.);
#5235=VECTOR('',#19641,6.);
#5236=VECTOR('',#19644,6.);
#5237=VECTOR('',#19647,6.);
#5238=VECTOR('',#19650,6.);
#5239=VECTOR('',#19653,6.);
#5240=VECTOR('',#19656,6.);
#5241=VECTOR('',#19659,6.);
#5242=VECTOR('',#19662,6.);
#5243=VECTOR('',#19665,6.);
#5244=VECTOR('',#19668,6.);
#5245=VECTOR('',#19671,6.);
#5246=VECTOR('',#19674,6.);
#5247=VECTOR('',#19677,6.);
#5248=VECTOR('',#19680,6.);
#5249=VECTOR('',#19683,6.);
#5250=VECTOR('',#19686,6.);
#5251=VECTOR('',#19689,6.);
#5252=VECTOR('',#19692,6.);
#5253=VECTOR('',#19695,6.);
#5254=VECTOR('',#19698,6.);
#5255=VECTOR('',#19701,6.);
#5256=VECTOR('',#19704,6.);
#5257=VECTOR('',#19707,6.);
#5258=VECTOR('',#19710,6.);
#5259=VECTOR('',#19713,6.);
#5260=VECTOR('',#19716,6.);
#5261=VECTOR('',#19719,4.91825);
#5262=VECTOR('',#19724,4.91825);
#5263=VECTOR('',#19727,4.91825);
#5264=VECTOR('',#19730,4.91825);
#5265=VECTOR('',#19733,4.91825);
#5266=VECTOR('',#19736,4.91825);
#5267=VECTOR('',#19739,4.91825);
#5268=VECTOR('',#19742,4.91825);
#5269=VECTOR('',#19745,4.91825);
#5270=VECTOR('',#19748,4.91825);
#5271=VECTOR('',#19751,4.91825);
#5272=VECTOR('',#19754,4.91825);
#5273=VECTOR('',#19757,4.91825);
#5274=VECTOR('',#19760,4.91825);
#5275=VECTOR('',#19763,4.91825);
#5276=VECTOR('',#19766,4.91825);
#5277=VECTOR('',#19769,4.91825);
#5278=VECTOR('',#19772,4.91825);
#5279=VECTOR('',#19775,4.91825);
#5280=VECTOR('',#19778,4.91825);
#5281=VECTOR('',#19781,4.91825);
#5282=VECTOR('',#19784,4.91825);
#5283=VECTOR('',#19787,4.91825);
#5284=VECTOR('',#19790,4.91825);
#5285=VECTOR('',#19793,4.91825);
#5286=VECTOR('',#19796,4.91825);
#5287=VECTOR('',#19799,4.91825);
#5288=VECTOR('',#19802,4.91825);
#5289=VECTOR('',#19805,4.91825);
#5290=VECTOR('',#19808,4.91825);
#5291=VECTOR('',#19811,4.91825);
#5292=VECTOR('',#19814,4.91825);
#5293=VECTOR('',#19817,4.91825);
#5294=VECTOR('',#19820,4.91825);
#5295=VECTOR('',#19833,10.);
#5296=VECTOR('',#19834,10.);
#5297=VECTOR('',#19835,10.);
#5298=VECTOR('',#19836,10.);
#5299=VECTOR('',#19841,10.);
#5300=VECTOR('',#19844,10.);
#5301=VECTOR('',#19845,10.);
#5302=VECTOR('',#19852,10.);
#5303=VECTOR('',#19853,10.);
#5304=VECTOR('',#19854,10.);
#5305=VECTOR('',#19855,10.);
#5306=VECTOR('',#19860,10.);
#5307=VECTOR('',#19863,10.);
#5308=VECTOR('',#19864,10.);
#5309=VECTOR('',#19871,10.);
#5310=VECTOR('',#19872,10.);
#5311=VECTOR('',#19873,10.);
#5312=VECTOR('',#19874,10.);
#5313=VECTOR('',#19879,10.);
#5314=VECTOR('',#19882,10.);
#5315=VECTOR('',#19883,10.);
#5316=VECTOR('',#19890,10.);
#5317=VECTOR('',#19891,10.);
#5318=VECTOR('',#19892,10.);
#5319=VECTOR('',#19893,10.);
#5320=VECTOR('',#19898,10.);
#5321=VECTOR('',#19901,10.);
#5322=VECTOR('',#19902,10.);
#5323=VECTOR('',#19909,10.);
#5324=VECTOR('',#19910,10.);
#5325=VECTOR('',#19911,10.);
#5326=VECTOR('',#19912,10.);
#5327=VECTOR('',#19917,10.);
#5328=VECTOR('',#19920,10.);
#5329=VECTOR('',#19921,10.);
#5330=VECTOR('',#19928,10.);
#5331=VECTOR('',#19929,10.);
#5332=VECTOR('',#19930,10.);
#5333=VECTOR('',#19931,10.);
#5334=VECTOR('',#19936,10.);
#5335=VECTOR('',#19939,10.);
#5336=VECTOR('',#19940,10.);
#5337=VECTOR('',#19947,10.);
#5338=VECTOR('',#19948,10.);
#5339=VECTOR('',#19949,10.);
#5340=VECTOR('',#19950,10.);
#5341=VECTOR('',#19955,10.);
#5342=VECTOR('',#19958,10.);
#5343=VECTOR('',#19959,10.);
#5344=VECTOR('',#19966,10.);
#5345=VECTOR('',#19967,10.);
#5346=VECTOR('',#19968,10.);
#5347=VECTOR('',#19969,10.);
#5348=VECTOR('',#19974,10.);
#5349=VECTOR('',#19977,10.);
#5350=VECTOR('',#19978,10.);
#5351=VECTOR('',#19985,10.);
#5352=VECTOR('',#19986,10.);
#5353=VECTOR('',#19987,10.);
#5354=VECTOR('',#19988,10.);
#5355=VECTOR('',#19993,10.);
#5356=VECTOR('',#19996,10.);
#5357=VECTOR('',#19997,10.);
#5358=VECTOR('',#20004,10.);
#5359=VECTOR('',#20005,10.);
#5360=VECTOR('',#20006,10.);
#5361=VECTOR('',#20007,10.);
#5362=VECTOR('',#20012,10.);
#5363=VECTOR('',#20015,10.);
#5364=VECTOR('',#20016,10.);
#5365=VECTOR('',#20023,10.);
#5366=VECTOR('',#20024,10.);
#5367=VECTOR('',#20025,10.);
#5368=VECTOR('',#20026,10.);
#5369=VECTOR('',#20031,10.);
#5370=VECTOR('',#20034,10.);
#5371=VECTOR('',#20035,10.);
#5372=VECTOR('',#20042,10.);
#5373=VECTOR('',#20043,10.);
#5374=VECTOR('',#20044,10.);
#5375=VECTOR('',#20045,10.);
#5376=VECTOR('',#20050,10.);
#5377=VECTOR('',#20053,10.);
#5378=VECTOR('',#20054,10.);
#5379=VECTOR('',#20061,10.);
#5380=VECTOR('',#20062,10.);
#5381=VECTOR('',#20063,10.);
#5382=VECTOR('',#20064,10.);
#5383=VECTOR('',#20069,10.);
#5384=VECTOR('',#20072,10.);
#5385=VECTOR('',#20073,10.);
#5386=VECTOR('',#20080,10.);
#5387=VECTOR('',#20081,10.);
#5388=VECTOR('',#20082,10.);
#5389=VECTOR('',#20083,10.);
#5390=VECTOR('',#20088,10.);
#5391=VECTOR('',#20091,10.);
#5392=VECTOR('',#20092,10.);
#5393=VECTOR('',#20099,10.);
#5394=VECTOR('',#20100,10.);
#5395=VECTOR('',#20101,10.);
#5396=VECTOR('',#20102,10.);
#5397=VECTOR('',#20107,10.);
#5398=VECTOR('',#20110,10.);
#5399=VECTOR('',#20111,10.);
#5400=VECTOR('',#20118,10.);
#5401=VECTOR('',#20119,10.);
#5402=VECTOR('',#20120,10.);
#5403=VECTOR('',#20121,10.);
#5404=VECTOR('',#20126,10.);
#5405=VECTOR('',#20129,10.);
#5406=VECTOR('',#20130,10.);
#5407=VECTOR('',#20137,10.);
#5408=VECTOR('',#20138,10.);
#5409=VECTOR('',#20139,10.);
#5410=VECTOR('',#20140,10.);
#5411=VECTOR('',#20145,10.);
#5412=VECTOR('',#20148,10.);
#5413=VECTOR('',#20149,10.);
#5414=VECTOR('',#20156,10.);
#5415=VECTOR('',#20157,10.);
#5416=VECTOR('',#20158,10.);
#5417=VECTOR('',#20159,10.);
#5418=VECTOR('',#20164,10.);
#5419=VECTOR('',#20169,10.);
#5420=VECTOR('',#20170,10.);
#5421=VECTOR('',#20179,10.);
#5422=VECTOR('',#20180,10.);
#5423=VECTOR('',#20181,10.);
#5424=VECTOR('',#20182,10.);
#5425=VECTOR('',#20187,10.);
#5426=VECTOR('',#20190,10.);
#5427=VECTOR('',#20191,10.);
#5428=VECTOR('',#20198,10.);
#5429=VECTOR('',#20199,10.);
#5430=VECTOR('',#20200,10.);
#5431=VECTOR('',#20201,10.);
#5432=VECTOR('',#20206,10.);
#5433=VECTOR('',#20209,10.);
#5434=VECTOR('',#20210,10.);
#5435=VECTOR('',#20217,10.);
#5436=VECTOR('',#20218,10.);
#5437=VECTOR('',#20219,10.);
#5438=VECTOR('',#20220,10.);
#5439=VECTOR('',#20225,10.);
#5440=VECTOR('',#20228,10.);
#5441=VECTOR('',#20229,10.);
#5442=VECTOR('',#20236,10.);
#5443=VECTOR('',#20237,10.);
#5444=VECTOR('',#20238,10.);
#5445=VECTOR('',#20239,10.);
#5446=VECTOR('',#20244,10.);
#5447=VECTOR('',#20247,10.);
#5448=VECTOR('',#20248,10.);
#5449=VECTOR('',#20255,10.);
#5450=VECTOR('',#20256,10.);
#5451=VECTOR('',#20257,10.);
#5452=VECTOR('',#20258,10.);
#5453=VECTOR('',#20263,10.);
#5454=VECTOR('',#20266,10.);
#5455=VECTOR('',#20267,10.);
#5456=VECTOR('',#20274,10.);
#5457=VECTOR('',#20275,10.);
#5458=VECTOR('',#20276,10.);
#5459=VECTOR('',#20277,10.);
#5460=VECTOR('',#20282,10.);
#5461=VECTOR('',#20285,10.);
#5462=VECTOR('',#20286,10.);
#5463=VECTOR('',#20293,10.);
#5464=VECTOR('',#20294,10.);
#5465=VECTOR('',#20295,10.);
#5466=VECTOR('',#20296,10.);
#5467=VECTOR('',#20301,10.);
#5468=VECTOR('',#20304,10.);
#5469=VECTOR('',#20305,10.);
#5470=VECTOR('',#20312,10.);
#5471=VECTOR('',#20313,10.);
#5472=VECTOR('',#20314,10.);
#5473=VECTOR('',#20315,10.);
#5474=VECTOR('',#20320,10.);
#5475=VECTOR('',#20323,10.);
#5476=VECTOR('',#20324,10.);
#5477=VECTOR('',#20331,10.);
#5478=VECTOR('',#20332,10.);
#5479=VECTOR('',#20333,10.);
#5480=VECTOR('',#20334,10.);
#5481=VECTOR('',#20339,10.);
#5482=VECTOR('',#20342,10.);
#5483=VECTOR('',#20343,10.);
#5484=VECTOR('',#20350,10.);
#5485=VECTOR('',#20351,10.);
#5486=VECTOR('',#20352,10.);
#5487=VECTOR('',#20353,10.);
#5488=VECTOR('',#20358,10.);
#5489=VECTOR('',#20361,10.);
#5490=VECTOR('',#20362,10.);
#5491=VECTOR('',#20369,10.);
#5492=VECTOR('',#20370,10.);
#5493=VECTOR('',#20371,10.);
#5494=VECTOR('',#20372,10.);
#5495=VECTOR('',#20377,10.);
#5496=VECTOR('',#20380,10.);
#5497=VECTOR('',#20381,10.);
#5498=VECTOR('',#20388,10.);
#5499=VECTOR('',#20389,10.);
#5500=VECTOR('',#20390,10.);
#5501=VECTOR('',#20391,10.);
#5502=VECTOR('',#20396,10.);
#5503=VECTOR('',#20399,10.);
#5504=VECTOR('',#20400,10.);
#5505=VECTOR('',#20407,10.);
#5506=VECTOR('',#20408,10.);
#5507=VECTOR('',#20409,10.);
#5508=VECTOR('',#20410,10.);
#5509=VECTOR('',#20415,10.);
#5510=VECTOR('',#20418,10.);
#5511=VECTOR('',#20419,10.);
#5512=VECTOR('',#20426,10.);
#5513=VECTOR('',#20427,10.);
#5514=VECTOR('',#20428,10.);
#5515=VECTOR('',#20429,10.);
#5516=VECTOR('',#20434,10.);
#5517=VECTOR('',#20437,10.);
#5518=VECTOR('',#20438,10.);
#5519=VECTOR('',#20445,10.);
#5520=VECTOR('',#20446,10.);
#5521=VECTOR('',#20447,10.);
#5522=VECTOR('',#20448,10.);
#5523=VECTOR('',#20453,10.);
#5524=VECTOR('',#20456,10.);
#5525=VECTOR('',#20457,10.);
#5526=VECTOR('',#20464,10.);
#5527=VECTOR('',#20465,10.);
#5528=VECTOR('',#20466,10.);
#5529=VECTOR('',#20467,10.);
#5530=VECTOR('',#20472,10.);
#5531=VECTOR('',#20475,10.);
#5532=VECTOR('',#20476,10.);
#5533=VECTOR('',#20483,10.);
#5534=VECTOR('',#20484,10.);
#5535=VECTOR('',#20485,10.);
#5536=VECTOR('',#20486,10.);
#5537=VECTOR('',#20491,10.);
#5538=VECTOR('',#20494,10.);
#5539=VECTOR('',#20495,10.);
#5540=VECTOR('',#20502,10.);
#5541=VECTOR('',#20503,10.);
#5542=VECTOR('',#20504,10.);
#5543=VECTOR('',#20505,10.);
#5544=VECTOR('',#20510,10.);
#5545=VECTOR('',#20513,10.);
#5546=VECTOR('',#20514,10.);
#5547=VECTOR('',#20521,10.);
#5548=VECTOR('',#20522,10.);
#5549=VECTOR('',#20523,10.);
#5550=VECTOR('',#20524,10.);
#5551=VECTOR('',#20527,10.);
#5552=VECTOR('',#20528,10.);
#5553=VECTOR('',#20529,10.);
#5554=VECTOR('',#20532,10.);
#5555=VECTOR('',#20533,10.);
#5556=VECTOR('',#20534,10.);
#5557=VECTOR('',#20537,10.);
#5558=VECTOR('',#20538,10.);
#5559=VECTOR('',#20539,10.);
#5560=VECTOR('',#20542,10.);
#5561=VECTOR('',#20543,10.);
#5562=VECTOR('',#20544,10.);
#5563=VECTOR('',#20547,10.);
#5564=VECTOR('',#20548,10.);
#5565=VECTOR('',#20557,5.75);
#5566=VECTOR('',#20570,9.);
#5567=VECTOR('',#20571,9.);
#5568=VECTOR('',#20576,8.75);
#5569=VECTOR('',#20583,9.);
#5570=VECTOR('',#20588,9.);
#5571=VECTOR('',#20591,9.);
#5572=VECTOR('',#20594,9.);
#5573=VECTOR('',#20597,9.);
#5574=VECTOR('',#20600,9.);
#5575=VECTOR('',#20603,9.);
#5576=VECTOR('',#20606,8.0685);
#5577=VECTOR('',#20611,8.0685);
#5578=VECTOR('',#20616,8.0685);
#5579=VECTOR('',#20619,8.0685);
#5580=VECTOR('',#20622,8.0685);
#5581=VECTOR('',#20625,8.0685);
#5582=VECTOR('',#20628,8.0685);
#5583=VECTOR('',#20631,10.);
#5584=VECTOR('',#20632,10.);
#5585=VECTOR('',#20633,10.);
#5586=VECTOR('',#20636,10.);
#5587=VECTOR('',#20637,10.);
#5588=VECTOR('',#20638,10.);
#5589=VECTOR('',#20641,10.);
#5590=VECTOR('',#20642,10.);
#5591=VECTOR('',#20643,10.);
#5592=VECTOR('',#20646,10.);
#5593=VECTOR('',#20647,10.);
#5594=VECTOR('',#20648,10.);
#5595=VECTOR('',#20651,10.);
#5596=VECTOR('',#20652,10.);
#5597=VECTOR('',#20655,10.);
#5598=VECTOR('',#20656,10.);
#5599=VECTOR('',#20657,10.);
#5600=VECTOR('',#20660,10.);
#5601=VECTOR('',#20661,10.);
#5602=VECTOR('',#20662,10.);
#5603=VECTOR('',#20665,10.);
#5604=VECTOR('',#20666,10.);
#5605=VECTOR('',#20667,10.);
#5606=VECTOR('',#20670,10.);
#5607=VECTOR('',#20671,10.);
#5608=VECTOR('',#20672,10.);
#5609=VECTOR('',#20675,10.);
#5610=VECTOR('',#20676,10.);
#5611=VECTOR('',#20679,10.);
#5612=VECTOR('',#20680,10.);
#5613=VECTOR('',#20681,10.);
#5614=VECTOR('',#20684,10.);
#5615=VECTOR('',#20685,10.);
#5616=VECTOR('',#20686,10.);
#5617=VECTOR('',#20689,10.);
#5618=VECTOR('',#20690,10.);
#5619=VECTOR('',#20691,10.);
#5620=VECTOR('',#20694,10.);
#5621=VECTOR('',#20695,10.);
#5622=VECTOR('',#20696,10.);
#5623=VECTOR('',#20699,10.);
#5624=VECTOR('',#20700,10.);
#5625=VECTOR('',#20703,10.);
#5626=VECTOR('',#20704,10.);
#5627=VECTOR('',#20707,10.);
#5628=VECTOR('',#20708,10.);
#5629=VECTOR('',#20711,10.);
#5630=VECTOR('',#20712,10.);
#5631=VECTOR('',#20715,10.);
#5632=VECTOR('',#20718,10.);
#5633=VECTOR('',#20721,10.);
#5634=VECTOR('',#20724,10.);
#5635=VECTOR('',#20725,10.);
#5636=VECTOR('',#20726,10.);
#5637=VECTOR('',#20727,10.);
#5638=VECTOR('',#20728,10.);
#5639=VECTOR('',#20729,10.);
#5640=VECTOR('',#20732,10.);
#5641=VECTOR('',#20733,10.);
#5642=VECTOR('',#20734,10.);
#5643=VECTOR('',#20737,10.);
#5644=VECTOR('',#20738,10.);
#5645=VECTOR('',#20741,10.);
#5646=VECTOR('',#20742,10.);
#5647=VECTOR('',#20743,10.);
#5648=VECTOR('',#20746,10.);
#5649=VECTOR('',#20747,10.);
#5650=VECTOR('',#20750,10.);
#5651=VECTOR('',#20753,10.);
#5652=VECTOR('',#20756,10.);
#5653=VECTOR('',#20757,10.);
#5654=VECTOR('',#20758,10.);
#5655=VECTOR('',#20761,10.);
#5656=VECTOR('',#20762,10.);
#5657=VECTOR('',#20765,10.);
#5658=VECTOR('',#20766,10.);
#5659=VECTOR('',#20785,10.);
#5660=VECTOR('',#20786,10.);
#5661=VECTOR('',#20789,10.);
#5662=VECTOR('',#20790,10.);
#5663=VECTOR('',#20793,10.);
#5664=VECTOR('',#20798,10.);
#5665=VECTOR('',#20801,10.);
#5666=VECTOR('',#20804,10.);
#5667=VECTOR('',#20817,12.5);
#5668=VECTOR('',#20824,8.75);
#5669=VECTOR('',#20829,8.);
#5670=CIRCLE('',#15255,14.5);
#5671=CIRCLE('',#15256,15.);
#5672=CIRCLE('',#15258,15.);
#5673=CIRCLE('',#15259,15.);
#5674=CIRCLE('',#15261,9.05);
#5675=CIRCLE('',#15263,7.65);
#5676=CIRCLE('',#15264,7.15);
#5677=CIRCLE('',#15266,62.);
#5678=CIRCLE('',#15267,62.);
#5679=CIRCLE('',#15268,12.);
#5680=CIRCLE('',#15270,7.15);
#5681=CIRCLE('',#15272,14.5);
#5682=CIRCLE('',#15273,15.);
#5683=CIRCLE('',#15275,9.55);
#5684=CIRCLE('',#15277,15.);
#5685=CIRCLE('',#15278,15.);
#5686=CIRCLE('',#15280,7.65);
#5687=CIRCLE('',#15281,7.15);
#5688=CIRCLE('',#15283,12.);
#5689=CIRCLE('',#15284,62.);
#5690=CIRCLE('',#15285,62.);
#5691=CIRCLE('',#15287,7.15);
#5692=CIRCLE('',#15289,9.05);
#5693=CIRCLE('',#15291,9.05);
#5694=CIRCLE('',#15293,6.55);
#5695=CIRCLE('',#15294,6.05);
#5696=CIRCLE('',#15296,26.);
#5697=CIRCLE('',#15297,26.);
#5698=CIRCLE('',#15298,26.);
#5699=CIRCLE('',#15299,26.);
#5700=CIRCLE('',#15300,6.55);
#5701=CIRCLE('',#15301,6.55);
#5702=CIRCLE('',#15302,52.);
#5703=CIRCLE('',#15303,6.55);
#5704=CIRCLE('',#15305,6.05);
#5705=CIRCLE('',#15307,6.05);
#5706=CIRCLE('',#15309,6.05);
#5707=CIRCLE('',#15311,6.05);
#5708=CIRCLE('',#15313,6.05);
#5709=CIRCLE('',#15315,6.05);
#5710=CIRCLE('',#15317,6.05);
#5711=CIRCLE('',#15319,62.5);
#5712=CIRCLE('',#15329,62.5);
#5713=CIRCLE('',#15333,62.5);
#5714=CIRCLE('',#15334,62.5);
#5715=CIRCLE('',#15335,62.5);
#5716=CIRCLE('',#15336,62.5);
#5717=CIRCLE('',#15338,62.5);
#5718=CIRCLE('',#15348,62.5);
#5719=CIRCLE('',#15352,62.5);
#5720=CIRCLE('',#15353,62.5);
#5721=CIRCLE('',#15354,62.5);
#5722=CIRCLE('',#15355,62.5);
#5723=CIRCLE('',#15357,7.65);
#5724=CIRCLE('',#15359,60.5);
#5725=CIRCLE('',#15360,12.);
#5726=CIRCLE('',#15361,60.5);
#5727=CIRCLE('',#15362,12.);
#5728=CIRCLE('',#15363,7.65);
#5729=CIRCLE('',#15364,50.8);
#5730=CIRCLE('',#15368,2.);
#5731=CIRCLE('',#15370,2.);
#5732=CIRCLE('',#15371,14.);
#5733=CIRCLE('',#15375,2.);
#5734=CIRCLE('',#15376,2.);
#5735=CIRCLE('',#15377,14.);
#5736=CIRCLE('',#15381,14.);
#5737=CIRCLE('',#15384,60.5);
#5738=CIRCLE('',#15386,2.);
#5739=CIRCLE('',#15388,2.);
#5740=CIRCLE('',#15389,14.);
#5741=CIRCLE('',#15395,60.5);
#5742=CIRCLE('',#15397,2.);
#5743=CIRCLE('',#15399,2.);
#5744=CIRCLE('',#15403,50.8);
#5745=CIRCLE('',#15404,2.);
#5746=CIRCLE('',#15405,50.3);
#5747=CIRCLE('',#15408,2.);
#5748=CIRCLE('',#15410,2.);
#5749=CIRCLE('',#15411,28.);
#5750=CIRCLE('',#15412,26.);
#5751=CIRCLE('',#15416,2.);
#5752=CIRCLE('',#15417,26.);
#5753=CIRCLE('',#15418,2.);
#5754=CIRCLE('',#15419,28.);
#5755=CIRCLE('',#15424,2.);
#5756=CIRCLE('',#15426,2.);
#5757=CIRCLE('',#15427,28.);
#5758=CIRCLE('',#15428,26.);
#5759=CIRCLE('',#15432,2.);
#5760=CIRCLE('',#15434,2.);
#5761=CIRCLE('',#15435,28.);
#5762=CIRCLE('',#15436,26.);
#5763=CIRCLE('',#15440,1.99999999999999);
#5764=CIRCLE('',#15441,2.);
#5765=CIRCLE('',#15443,2.);
#5766=CIRCLE('',#15444,28.);
#5767=CIRCLE('',#15446,2.);
#5768=CIRCLE('',#15448,2.);
#5769=CIRCLE('',#15449,28.);
#5770=CIRCLE('',#15451,2.);
#5771=CIRCLE('',#15453,2.);
#5772=CIRCLE('',#15454,28.);
#5773=CIRCLE('',#15456,2.);
#5774=CIRCLE('',#15458,28.);
#5775=CIRCLE('',#15462,2.);
#5776=CIRCLE('',#15463,50.);
#5777=CIRCLE('',#15464,50.);
#5778=CIRCLE('',#15466,50.);
#5779=CIRCLE('',#15467,2.00000000000001);
#5780=CIRCLE('',#15468,2.);
#5781=CIRCLE('',#15469,1.99999999999999);
#5782=CIRCLE('',#15470,1.99999999999999);
#5783=CIRCLE('',#15471,9.05);
#5784=CIRCLE('',#15478,23.525);
#5785=CIRCLE('',#15479,23.525);
#5786=CIRCLE('',#15481,27.505);
#5787=CIRCLE('',#15483,27.505);
#5788=CIRCLE('',#15485,26.);
#5789=CIRCLE('',#15487,26.);
#5790=CIRCLE('',#15496,13.5);
#5791=CIRCLE('',#15497,13.);
#5792=CIRCLE('',#15498,13.);
#5793=CIRCLE('',#15500,16.505);
#5794=CIRCLE('',#15502,13.);
#5795=CIRCLE('',#15504,19.5);
#5796=CIRCLE('',#15505,19.);
#5797=CIRCLE('',#15507,6.54999999999999);
#5798=CIRCLE('',#15508,6.55);
#5799=CIRCLE('',#15509,6.55);
#5800=CIRCLE('',#15510,6.54999999999999);
#5801=CIRCLE('',#15512,19.);
#5802=CIRCLE('',#15514,6.05);
#5803=CIRCLE('',#15515,6.05);
#5804=CIRCLE('',#15517,6.05);
#5805=CIRCLE('',#15518,6.54999999999999);
#5806=CIRCLE('',#15521,2.00000000000001);
#5807=CIRCLE('',#15522,2.00000000000001);
#5808=CIRCLE('',#15524,6.05);
#5809=CIRCLE('',#15526,6.05);
#5810=CIRCLE('',#15528,6.05);
#5811=CIRCLE('',#15529,6.55);
#5812=CIRCLE('',#15532,2.);
#5813=CIRCLE('',#15533,2.00000000000001);
#5814=CIRCLE('',#15535,6.05);
#5815=CIRCLE('',#15537,6.05);
#5816=CIRCLE('',#15538,6.54999999999999);
#5817=CIRCLE('',#15540,6.05);
#5818=CIRCLE('',#15541,6.05);
#5819=CIRCLE('',#15543,6.05);
#5820=CIRCLE('',#15545,6.05);
#5821=CIRCLE('',#15547,6.05);
#5822=CIRCLE('',#15548,6.55);
#5823=CIRCLE('',#15551,2.);
#5824=CIRCLE('',#15552,1.99999999999999);
#5825=CIRCLE('',#15554,6.05);
#5826=CIRCLE('',#15556,2.);
#5827=CIRCLE('',#15557,1.5);
#5828=CIRCLE('',#15559,2.);
#5829=CIRCLE('',#15561,2.);
#5830=CIRCLE('',#15562,1.5);
#5831=CIRCLE('',#15564,12.);
#5832=CIRCLE('',#15565,1.99999999999999);
#5833=CIRCLE('',#15566,10.);
#5834=CIRCLE('',#15568,12.);
#5835=CIRCLE('',#15569,26.);
#5836=CIRCLE('',#15570,26.);
#5837=CIRCLE('',#15571,12.);
#5838=CIRCLE('',#15572,26.);
#5839=CIRCLE('',#15573,26.);
#5840=CIRCLE('',#15574,12.);
#5841=CIRCLE('',#15575,26.);
#5842=CIRCLE('',#15576,26.);
#5843=CIRCLE('',#15578,5.55000000000001);
#5844=CIRCLE('',#15579,5.05000000000001);
#5845=CIRCLE('',#15581,5.55);
#5846=CIRCLE('',#15582,5.55000000000001);
#5847=CIRCLE('',#15583,10.);
#5848=CIRCLE('',#15584,5.55);
#5849=CIRCLE('',#15586,5.05000000000001);
#5850=CIRCLE('',#15588,5.04999999999999);
#5851=CIRCLE('',#15590,5.04999999999999);
#5852=CIRCLE('',#15592,5.04999999999999);
#5853=CIRCLE('',#15594,5.04999999999999);
#5854=CIRCLE('',#15596,5.05000000000001);
#5855=CIRCLE('',#15598,5.05000000000001);
#5856=CIRCLE('',#15600,9.49999999999999);
#5857=CIRCLE('',#15602,9.49999999999999);
#5858=CIRCLE('',#15603,2.00000000000001);
#5859=CIRCLE('',#15605,6.);
#5860=CIRCLE('',#15607,2.00000000000001);
#5861=CIRCLE('',#15609,2.);
#5862=CIRCLE('',#15610,1.99999999999999);
#5863=CIRCLE('',#15611,2.);
#5864=CIRCLE('',#15613,2.);
#5865=CIRCLE('',#15616,2.);
#5866=CIRCLE('',#15618,2.);
#5867=CIRCLE('',#15620,1.99999999999999);
#5868=CIRCLE('',#15622,2.);
#5869=CIRCLE('',#15625,2.);
#5870=CIRCLE('',#15627,2.);
#5871=CIRCLE('',#15629,1.99999999999999);
#5872=CIRCLE('',#15631,2.);
#5873=CIRCLE('',#15632,1.99999999999999);
#5874=CIRCLE('',#15635,2.);
#5875=CIRCLE('',#15637,2.00000000000001);
#5876=CIRCLE('',#15639,2.00000000000001);
#5877=CIRCLE('',#15645,26.);
#5878=CIRCLE('',#15646,26.);
#5879=CIRCLE('',#15647,26.);
#5880=CIRCLE('',#15648,26.);
#5881=CIRCLE('',#15649,45.05);
#5882=CIRCLE('',#15650,6.5);
#5883=CIRCLE('',#15651,6.5);
#5884=CIRCLE('',#15652,6.5);
#5885=CIRCLE('',#15653,6.5);
#5886=CIRCLE('',#15655,2.);
#5887=CIRCLE('',#15656,43.05);
#5888=CIRCLE('',#15657,43.05);
#5889=CIRCLE('',#15659,43.05);
#5890=CIRCLE('',#15661,1.99999999999999);
#5891=CIRCLE('',#15662,28.);
#5892=CIRCLE('',#15664,1.99999999999999);
#5893=CIRCLE('',#15666,28.);
#5894=CIRCLE('',#15667,1.99999999999999);
#5895=CIRCLE('',#15668,1.99999999999999);
#5896=CIRCLE('',#15670,16.6);
#5897=CIRCLE('',#15672,28.);
#5898=CIRCLE('',#15673,26.);
#5899=CIRCLE('',#15675,2.);
#5900=CIRCLE('',#15676,10.);
#5901=CIRCLE('',#15677,6.5);
#5902=CIRCLE('',#15679,26.);
#5903=CIRCLE('',#15680,28.);
#5904=CIRCLE('',#15682,28.);
#5905=CIRCLE('',#15683,28.);
#5906=CIRCLE('',#15685,26.);
#5907=CIRCLE('',#15686,28.);
#5908=CIRCLE('',#15688,2.);
#5909=CIRCLE('',#15689,10.);
#5910=CIRCLE('',#15690,2.);
#5911=CIRCLE('',#15691,6.5);
#5912=CIRCLE('',#15693,26.);
#5913=CIRCLE('',#15694,28.);
#5914=CIRCLE('',#15696,2.);
#5915=CIRCLE('',#15697,10.);
#5916=CIRCLE('',#15698,2.);
#5917=CIRCLE('',#15699,6.5);
#5918=CIRCLE('',#15701,2.);
#5919=CIRCLE('',#15702,1.99999999999999);
#5920=CIRCLE('',#15705,28.);
#5921=CIRCLE('',#15707,28.);
#5922=CIRCLE('',#15708,28.);
#5923=CIRCLE('',#15711,2.);
#5924=CIRCLE('',#15712,2.00000000000003);
#5925=CIRCLE('',#15713,28.);
#5926=CIRCLE('',#15715,2.);
#5927=CIRCLE('',#15717,2.00000000000001);
#5928=CIRCLE('',#15718,28.);
#5929=CIRCLE('',#15720,2.);
#5930=CIRCLE('',#15721,2.);
#5931=CIRCLE('',#15723,2.);
#5932=CIRCLE('',#15724,2.);
#5933=CIRCLE('',#15726,10.);
#5934=CIRCLE('',#15727,2.00000000000001);
#5935=CIRCLE('',#15730,28.);
#5936=CIRCLE('',#15736,2.);
#5937=CIRCLE('',#15739,10.);
#5938=CIRCLE('',#15742,2.);
#5939=CIRCLE('',#15744,10.);
#5940=CIRCLE('',#15746,2.00000000000001);
#5941=CIRCLE('',#15747,1.99999999999999);
#5942=CIRCLE('',#15748,2.00000000000001);
#5943=CIRCLE('',#15750,2.00000000000001);
#5944=CIRCLE('',#15751,1.99999999999999);
#5945=CIRCLE('',#15752,2.00000000000001);
#5946=CIRCLE('',#15754,2.00000000000001);
#5947=CIRCLE('',#15755,2.00000000000001);
#5948=CIRCLE('',#15757,2.);
#5949=CIRCLE('',#15759,2.);
#5950=CIRCLE('',#15762,2.);
#5951=CIRCLE('',#15764,10.);
#5952=CIRCLE('',#15770,2.00000000000001);
#5953=CIRCLE('',#15771,1.99999999999999);
#5954=CIRCLE('',#15776,6.5);
#5955=CIRCLE('',#15793,16.6);
#5956=CIRCLE('',#15795,16.505);
#5957=CIRCLE('',#15805,48.);
#5958=CIRCLE('',#15818,48.);
#5959=CIRCLE('',#15819,20.);
#5960=CIRCLE('',#15827,41.8535533905933);
#5961=CIRCLE('',#15828,41.8535533905933);
#5962=CIRCLE('',#15829,41.);
#5963=CIRCLE('',#15831,8.51);
#5964=CIRCLE('',#15832,8.51);
#5965=CIRCLE('',#15833,8.51);
#5966=CIRCLE('',#15834,8.51);
#5967=CIRCLE('',#15835,8.51);
#5968=CIRCLE('',#15836,8.51);
#5969=CIRCLE('',#15837,8.51);
#5970=CIRCLE('',#15838,12.51);
#5971=CIRCLE('',#15840,42.5);
#5972=CIRCLE('',#15850,12.51);
#5973=CIRCLE('',#15857,42.5);
#5974=CIRCLE('',#15858,5.);
#5975=CIRCLE('',#15859,5.);
#5976=CIRCLE('',#15860,5.);
#5977=CIRCLE('',#15861,5.);
#5978=CIRCLE('',#15862,5.);
#5979=CIRCLE('',#15863,5.);
#5980=CIRCLE('',#15864,5.);
#5981=CIRCLE('',#15866,5.);
#5982=CIRCLE('',#15868,8.51);
#5983=CIRCLE('',#15871,5.);
#5984=CIRCLE('',#15873,8.51);
#5985=CIRCLE('',#15876,5.);
#5986=CIRCLE('',#15878,8.51);
#5987=CIRCLE('',#15881,5.);
#5988=CIRCLE('',#15883,8.51);
#5989=CIRCLE('',#15886,5.);
#5990=CIRCLE('',#15888,8.51);
#5991=CIRCLE('',#15891,5.);
#5992=CIRCLE('',#15893,8.51);
#5993=CIRCLE('',#15896,5.);
#5994=CIRCLE('',#15898,8.51);
#5995=CIRCLE('',#15931,33.);
#5996=CIRCLE('',#15932,33.);
#5997=CIRCLE('',#15934,23.);
#5998=CIRCLE('',#15935,23.);
#5999=CIRCLE('',#15937,33.);
#6000=CIRCLE('',#15938,33.);
#6001=CIRCLE('',#15940,23.);
#6002=CIRCLE('',#15941,23.);
#6003=CIRCLE('',#15943,15.5);
#6004=CIRCLE('',#15944,15.5);
#6005=CIRCLE('',#15946,43.);
#6006=CIRCLE('',#15948,43.);
#6007=CIRCLE('',#15954,11.1);
#6008=CIRCLE('',#15955,10.6);
#6009=CIRCLE('',#15962,11.1);
#6010=CIRCLE('',#15963,10.6);
#6011=CIRCLE('',#15970,11.1);
#6012=CIRCLE('',#15971,10.6);
#6013=CIRCLE('',#15978,11.1);
#6014=CIRCLE('',#15979,10.6);
#6015=CIRCLE('',#15987,10.6);
#6016=CIRCLE('',#15988,11.1);
#6017=CIRCLE('',#15991,11.1);
#6018=CIRCLE('',#15992,10.6);
#6019=CIRCLE('',#15994,11.1);
#6020=CIRCLE('',#15995,11.1);
#6021=CIRCLE('',#15996,11.1);
#6022=CIRCLE('',#15997,11.1);
#6023=CIRCLE('',#15998,11.1);
#6024=CIRCLE('',#15999,11.1);
#6025=CIRCLE('',#16000,11.1);
#6026=CIRCLE('',#16001,11.1);
#6027=CIRCLE('',#16002,11.1);
#6028=CIRCLE('',#16003,11.1);
#6029=CIRCLE('',#16004,11.1);
#6030=CIRCLE('',#16005,11.1);
#6031=CIRCLE('',#16006,11.1);
#6032=CIRCLE('',#16007,11.1);
#6033=CIRCLE('',#16008,11.1);
#6034=CIRCLE('',#16009,11.1);
#6035=CIRCLE('',#16010,11.1);
#6036=CIRCLE('',#16011,11.1);
#6037=CIRCLE('',#16012,11.1);
#6038=CIRCLE('',#16013,11.1);
#6039=CIRCLE('',#16014,11.1);
#6040=CIRCLE('',#16015,11.1);
#6041=CIRCLE('',#16019,10.6);
#6042=CIRCLE('',#16026,10.6);
#6043=CIRCLE('',#16057,10.6);
#6044=CIRCLE('',#16064,10.6);
#6045=CIRCLE('',#16071,10.6);
#6046=CIRCLE('',#16078,10.6);
#6047=CIRCLE('',#16085,10.6);
#6048=CIRCLE('',#16089,10.6);
#6049=CIRCLE('',#16095,10.6);
#6050=CIRCLE('',#16099,10.6);
#6051=CIRCLE('',#16101,3.85);
#6052=CIRCLE('',#16102,3.35);
#6053=CIRCLE('',#16104,3.35);
#6054=CIRCLE('',#16106,10.6);
#6055=CIRCLE('',#16107,10.6);
#6056=CIRCLE('',#16108,10.6);
#6057=CIRCLE('',#16109,10.6);
#6058=CIRCLE('',#16110,10.6);
#6059=CIRCLE('',#16111,10.6);
#6060=CIRCLE('',#16112,10.6);
#6061=CIRCLE('',#16113,10.6);
#6062=CIRCLE('',#16114,10.6);
#6063=CIRCLE('',#16115,10.6);
#6064=CIRCLE('',#16118,12.5);
#6065=CIRCLE('',#16122,12.5);
#6066=CIRCLE('',#16138,15.);
#6067=CIRCLE('',#16140,15.);
#6068=CIRCLE('',#16142,14.);
#6069=CIRCLE('',#16144,14.);
#6070=CIRCLE('',#16146,12.5);
#6071=CIRCLE('',#16148,12.5);
#6072=CIRCLE('',#16150,12.);
#6073=CIRCLE('',#16173,19.3);
#6074=CIRCLE('',#16174,19.);
#6075=CIRCLE('',#16176,23.8);
#6076=CIRCLE('',#16178,24.);
#6077=CIRCLE('',#16180,27.1);
#6078=CIRCLE('',#16182,27.5);
#6079=CIRCLE('',#16184,27.5);
#6080=CIRCLE('',#16186,27.1);
#6081=CIRCLE('',#16188,24.);
#6082=CIRCLE('',#16190,23.8);
#6083=CIRCLE('',#16192,19.3);
#6084=CIRCLE('',#16194,19.);
#6085=CIRCLE('',#16196,15.4);
#6086=CIRCLE('',#16198,15.);
#6087=CIRCLE('',#16200,15.);
#6088=CIRCLE('',#16202,15.4);
#6089=CIRCLE('',#16206,12.5);
#6090=CIRCLE('',#16207,12.5);
#6091=CIRCLE('',#16209,15.6);
#6092=CIRCLE('',#16211,15.6);
#6093=CIRCLE('',#16213,15.6);
#6094=CIRCLE('',#16215,13.5);
#6095=CIRCLE('',#16216,13.5);
#6096=CIRCLE('',#16218,16.5);
#6097=CIRCLE('',#16220,16.5);
#6098=CIRCLE('',#16222,13.5);
#6099=CIRCLE('',#16224,13.5);
#6100=CIRCLE('',#16227,15.6);
#6101=CIRCLE('',#16231,20.5);
#6102=CIRCLE('',#16232,20.5);
#6103=CIRCLE('',#16233,20.78);
#6104=CIRCLE('',#16235,23.52);
#6105=CIRCLE('',#16237,20.5);
#6106=CIRCLE('',#16239,17.2329740824146);
#6107=CIRCLE('',#16240,17.2329740824146);
#6108=CIRCLE('',#16241,16.72);
#6109=CIRCLE('',#16243,15.);
#6110=CIRCLE('',#16245,18.5);
#6111=CIRCLE('',#16247,15.);
#6112=CIRCLE('',#16249,23.52);
#6113=CIRCLE('',#16252,18.);
#6114=CIRCLE('',#16256,4.5);
#6115=CIRCLE('',#16257,4.);
#6116=CIRCLE('',#16259,4.);
#6117=CIRCLE('',#16261,8.);
#6118=CIRCLE('',#16263,1.);
#6119=CIRCLE('',#16264,1.);
#6120=CIRCLE('',#16265,1.);
#6121=CIRCLE('',#16268,4.);
#6122=CIRCLE('',#16269,4.);
#6123=CIRCLE('',#16270,4.);
#6124=CIRCLE('',#16272,8.);
#6125=CIRCLE('',#16274,8.5);
#6126=CIRCLE('',#16276,8.5);
#6127=CIRCLE('',#16278,6.99981782686978);
#6128=CIRCLE('',#16281,5.);
#6129=CIRCLE('',#16282,5.);
#6130=CIRCLE('',#16284,10.5);
#6131=CIRCLE('',#16286,11.);
#6132=CIRCLE('',#16288,11.);
#6133=CIRCLE('',#16290,9.);
#6134=CIRCLE('',#16292,9.);
#6135=CIRCLE('',#16294,6.08526088183572);
#6136=CIRCLE('',#16296,2.);
#6137=CIRCLE('',#16297,7.02);
#6138=CIRCLE('',#16298,2.);
#6139=CIRCLE('',#16299,2.);
#6140=CIRCLE('',#16300,7.02);
#6141=CIRCLE('',#16302,2.);
#6142=CIRCLE('',#16306,40.8);
#6143=CIRCLE('',#16307,41.);
#6144=CIRCLE('',#16308,41.);
#6145=CIRCLE('',#16310,10.5);
#6146=CIRCLE('',#16311,22.);
#6147=CIRCLE('',#16312,10.5);
#6148=CIRCLE('',#16313,22.);
#6149=CIRCLE('',#16314,10.5);
#6150=CIRCLE('',#16315,22.);
#6151=CIRCLE('',#16316,10.5);
#6152=CIRCLE('',#16317,22.);
#6153=CIRCLE('',#16318,10.5);
#6154=CIRCLE('',#16319,22.);
#6155=CIRCLE('',#16320,10.5);
#6156=CIRCLE('',#16321,22.);
#6157=CIRCLE('',#16322,10.5);
#6158=CIRCLE('',#16323,22.);
#6159=CIRCLE('',#16325,41.);
#6160=CIRCLE('',#16327,10.5);
#6161=CIRCLE('',#16329,22.);
#6162=CIRCLE('',#16331,10.5);
#6163=CIRCLE('',#16333,22.);
#6164=CIRCLE('',#16335,10.5);
#6165=CIRCLE('',#16337,22.);
#6166=CIRCLE('',#16339,10.5);
#6167=CIRCLE('',#16341,22.);
#6168=CIRCLE('',#16343,10.5);
#6169=CIRCLE('',#16345,22.);
#6170=CIRCLE('',#16347,10.5);
#6171=CIRCLE('',#16349,22.);
#6172=CIRCLE('',#16351,10.5);
#6173=CIRCLE('',#16353,40.5);
#6174=CIRCLE('',#16354,22.);
#6175=CIRCLE('',#16359,5.91675);
#6176=CIRCLE('',#16394,4.91825);
#6177=CIRCLE('',#16429,5.91675);
#6178=CIRCLE('',#16430,5.91675);
#6179=CIRCLE('',#16431,4.91825);
#6180=CIRCLE('',#16435,9.);
#6181=CIRCLE('',#16438,9.);
#6182=CIRCLE('',#16441,9.);
#6183=CIRCLE('',#16444,9.);
#6184=CIRCLE('',#16447,9.);
#6185=CIRCLE('',#16450,9.);
#6186=CIRCLE('',#16453,9.);
#6187=CIRCLE('',#16456,9.);
#6188=CIRCLE('',#16459,9.);
#6189=CIRCLE('',#16462,9.);
#6190=CIRCLE('',#16465,9.);
#6191=CIRCLE('',#16468,9.);
#6192=CIRCLE('',#16471,9.);
#6193=CIRCLE('',#16474,9.);
#6194=CIRCLE('',#16477,9.);
#6195=CIRCLE('',#16480,9.);
#6196=CIRCLE('',#16483,9.);
#6197=CIRCLE('',#16486,9.);
#6198=CIRCLE('',#16489,9.);
#6199=CIRCLE('',#16492,9.);
#6200=CIRCLE('',#16495,9.);
#6201=CIRCLE('',#16498,9.);
#6202=CIRCLE('',#16501,9.);
#6203=CIRCLE('',#16504,9.);
#6204=CIRCLE('',#16507,9.);
#6205=CIRCLE('',#16510,9.);
#6206=CIRCLE('',#16513,9.);
#6207=CIRCLE('',#16516,9.);
#6208=CIRCLE('',#16519,9.);
#6209=CIRCLE('',#16522,9.);
#6210=CIRCLE('',#16525,9.);
#6211=CIRCLE('',#16528,9.);
#6212=CIRCLE('',#16531,9.);
#6213=CIRCLE('',#16534,9.);
#6214=CIRCLE('',#16537,9.);
#6215=CIRCLE('',#16538,9.);
#6216=CIRCLE('',#16541,9.);
#6217=CIRCLE('',#16542,9.);
#6218=CIRCLE('',#16545,9.);
#6219=CIRCLE('',#16548,9.);
#6220=CIRCLE('',#16551,9.);
#6221=CIRCLE('',#16554,9.);
#6222=CIRCLE('',#16557,9.);
#6223=CIRCLE('',#16560,9.);
#6224=CIRCLE('',#16563,9.);
#6225=CIRCLE('',#16566,9.);
#6226=CIRCLE('',#16569,9.);
#6227=CIRCLE('',#16572,9.);
#6228=CIRCLE('',#16575,9.);
#6229=CIRCLE('',#16578,9.);
#6230=CIRCLE('',#16581,9.);
#6231=CIRCLE('',#16584,9.);
#6232=CIRCLE('',#16587,9.);
#6233=CIRCLE('',#16590,9.);
#6234=CIRCLE('',#16593,9.);
#6235=CIRCLE('',#16596,9.);
#6236=CIRCLE('',#16599,9.);
#6237=CIRCLE('',#16602,9.);
#6238=CIRCLE('',#16605,9.);
#6239=CIRCLE('',#16608,9.);
#6240=CIRCLE('',#16611,9.);
#6241=CIRCLE('',#16614,9.);
#6242=CIRCLE('',#16617,9.);
#6243=CIRCLE('',#16620,9.);
#6244=CIRCLE('',#16623,9.);
#6245=CIRCLE('',#16626,9.);
#6246=CIRCLE('',#16629,9.);
#6247=CIRCLE('',#16632,9.);
#6248=CIRCLE('',#16635,9.);
#6249=CIRCLE('',#16638,9.);
#6250=CIRCLE('',#16641,9.);
#6251=CIRCLE('',#16644,9.);
#6252=CIRCLE('',#16647,9.);
#6253=CIRCLE('',#16650,9.);
#6254=CIRCLE('',#16659,5.5);
#6255=CIRCLE('',#16662,5.91675);
#6256=CIRCLE('',#16664,9.);
#6257=CIRCLE('',#16666,9.);
#6258=CIRCLE('',#16668,8.5);
#6259=CIRCLE('',#16672,8.925);
#6260=CIRCLE('',#16680,8.0685);
#6261=CIRCLE('',#16682,8.0685);
#6262=CIRCLE('',#16720,8.925);
#6263=CIRCLE('',#16721,8.925);
#6264=CIRCLE('',#16722,8.0685);
#6265=CIRCLE('',#16725,8.925);
#6266=CIRCLE('',#16726,8.);
#6267=CIRCLE('',#16735,12.5);
#6268=CIRCLE('',#16737,12.5);
#6269=CIRCLE('',#16738,8.);
#6270=CIRCLE('',#16741,8.5);
#6271=VERTEX_POINT('',#20893);
#6272=VERTEX_POINT('',#20895);
#6273=VERTEX_POINT('',#20899);
#6274=VERTEX_POINT('',#20901);
#6275=VERTEX_POINT('',#20903);
#6276=VERTEX_POINT('',#20916);
#6277=VERTEX_POINT('',#20919);
#6278=VERTEX_POINT('',#20921);
#6279=VERTEX_POINT('',#20925);
#6280=VERTEX_POINT('',#20926);
#6281=VERTEX_POINT('',#20928);
#6282=VERTEX_POINT('',#20930);
#6283=VERTEX_POINT('',#20932);
#6284=VERTEX_POINT('',#20934);
#6285=VERTEX_POINT('',#20938);
#6286=VERTEX_POINT('',#20942);
#6287=VERTEX_POINT('',#20944);
#6288=VERTEX_POINT('',#20948);
#6289=VERTEX_POINT('',#20951);
#6290=VERTEX_POINT('',#20953);
#6291=VERTEX_POINT('',#20955);
#6292=VERTEX_POINT('',#20968);
#6293=VERTEX_POINT('',#20970);
#6294=VERTEX_POINT('',#20974);
#6295=VERTEX_POINT('',#20975);
#6296=VERTEX_POINT('',#20977);
#6297=VERTEX_POINT('',#20979);
#6298=VERTEX_POINT('',#20981);
#6299=VERTEX_POINT('',#20983);
#6300=VERTEX_POINT('',#20987);
#6301=VERTEX_POINT('',#20991);
#6302=VERTEX_POINT('',#20995);
#6303=VERTEX_POINT('',#20997);
#6304=VERTEX_POINT('',#21003);
#6305=VERTEX_POINT('',#21015);
#6306=VERTEX_POINT('',#21017);
#6307=VERTEX_POINT('',#21021);
#6308=VERTEX_POINT('',#21022);
#6309=VERTEX_POINT('',#21024);
#6310=VERTEX_POINT('',#21026);
#6311=VERTEX_POINT('',#21028);
#6312=VERTEX_POINT('',#21030);
#6313=VERTEX_POINT('',#21032);
#6314=VERTEX_POINT('',#21034);
#6315=VERTEX_POINT('',#21037);
#6316=VERTEX_POINT('',#21039);
#6317=VERTEX_POINT('',#21041);
#6318=VERTEX_POINT('',#21043);
#6319=VERTEX_POINT('',#21046);
#6320=VERTEX_POINT('',#21050);
#6321=VERTEX_POINT('',#21054);
#6322=VERTEX_POINT('',#21058);
#6323=VERTEX_POINT('',#21062);
#6324=VERTEX_POINT('',#21066);
#6325=VERTEX_POINT('',#21070);
#6326=VERTEX_POINT('',#21074);
#6327=VERTEX_POINT('',#21083);
#6328=VERTEX_POINT('',#21085);
#6329=VERTEX_POINT('',#21094);
#6330=VERTEX_POINT('',#21096);
#6331=VERTEX_POINT('',#21100);
#6332=VERTEX_POINT('',#21102);
#6333=VERTEX_POINT('',#21104);
#6334=VERTEX_POINT('',#21106);
#6335=VERTEX_POINT('',#21108);
#6336=VERTEX_POINT('',#21110);
#6337=VERTEX_POINT('',#21116);
#6338=VERTEX_POINT('',#21117);
#6339=VERTEX_POINT('',#21128);
#6340=VERTEX_POINT('',#21130);
#6341=VERTEX_POINT('',#21134);
#6342=VERTEX_POINT('',#21136);
#6343=VERTEX_POINT('',#21147);
#6344=VERTEX_POINT('',#21149);
#6345=VERTEX_POINT('',#21160);
#6346=VERTEX_POINT('',#21162);
#6347=VERTEX_POINT('',#21165);
#6348=VERTEX_POINT('',#21167);
#6349=VERTEX_POINT('',#21171);
#6350=VERTEX_POINT('',#21173);
#6351=VERTEX_POINT('',#21186);
#6352=VERTEX_POINT('',#21187);
#6353=VERTEX_POINT('',#21197);
#6354=VERTEX_POINT('',#21206);
#6355=VERTEX_POINT('',#21208);
#6356=VERTEX_POINT('',#21212);
#6357=VERTEX_POINT('',#21221);
#6358=VERTEX_POINT('',#21223);
#6359=VERTEX_POINT('',#21225);
#6360=VERTEX_POINT('',#21235);
#6361=VERTEX_POINT('',#21244);
#6362=VERTEX_POINT('',#21255);
#6363=VERTEX_POINT('',#21264);
#6364=VERTEX_POINT('',#21275);
#6365=VERTEX_POINT('',#21284);
#6366=VERTEX_POINT('',#21286);
#6367=VERTEX_POINT('',#21295);
#6368=VERTEX_POINT('',#21297);
#6369=VERTEX_POINT('',#21301);
#6370=VERTEX_POINT('',#21303);
#6371=VERTEX_POINT('',#21305);
#6372=VERTEX_POINT('',#21307);
#6373=VERTEX_POINT('',#21311);
#6374=VERTEX_POINT('',#21312);
#6375=VERTEX_POINT('',#21323);
#6376=VERTEX_POINT('',#21325);
#6377=VERTEX_POINT('',#21329);
#6378=VERTEX_POINT('',#21331);
#6379=VERTEX_POINT('',#21342);
#6380=VERTEX_POINT('',#21344);
#6381=VERTEX_POINT('',#21355);
#6382=VERTEX_POINT('',#21357);
#6383=VERTEX_POINT('',#21359);
#6384=VERTEX_POINT('',#21361);
#6385=VERTEX_POINT('',#21366);
#6386=VERTEX_POINT('',#21368);
#6387=VERTEX_POINT('',#21381);
#6388=VERTEX_POINT('',#21382);
#6389=VERTEX_POINT('',#21397);
#6390=VERTEX_POINT('',#21401);
#6391=VERTEX_POINT('',#21410);
#6392=VERTEX_POINT('',#21412);
#6393=VERTEX_POINT('',#21414);
#6394=VERTEX_POINT('',#21424);
#6395=VERTEX_POINT('',#21433);
#6396=VERTEX_POINT('',#21444);
#6397=VERTEX_POINT('',#21453);
#6398=VERTEX_POINT('',#21464);
#6399=VERTEX_POINT('',#21468);
#6400=VERTEX_POINT('',#21469);
#6401=VERTEX_POINT('',#21471);
#6402=VERTEX_POINT('',#21473);
#6403=VERTEX_POINT('',#21475);
#6404=VERTEX_POINT('',#21477);
#6405=VERTEX_POINT('',#21479);
#6406=VERTEX_POINT('',#21481);
#6407=VERTEX_POINT('',#21484);
#6408=VERTEX_POINT('',#21486);
#6409=VERTEX_POINT('',#21520);
#6410=VERTEX_POINT('',#21524);
#6411=VERTEX_POINT('',#21559);
#6412=VERTEX_POINT('',#21561);
#6413=VERTEX_POINT('',#21569);
#6414=VERTEX_POINT('',#21571);
#6415=VERTEX_POINT('',#21579);
#6416=VERTEX_POINT('',#21583);
#6417=VERTEX_POINT('',#21603);
#6418=VERTEX_POINT('',#21605);
#6419=VERTEX_POINT('',#21611);
#6420=VERTEX_POINT('',#21615);
#6421=VERTEX_POINT('',#21623);
#6422=VERTEX_POINT('',#21625);
#6423=VERTEX_POINT('',#21635);
#6424=VERTEX_POINT('',#21639);
#6425=VERTEX_POINT('',#21647);
#6426=VERTEX_POINT('',#21651);
#6427=VERTEX_POINT('',#21681);
#6428=VERTEX_POINT('',#21683);
#6429=VERTEX_POINT('',#21687);
#6430=VERTEX_POINT('',#21690);
#6431=VERTEX_POINT('',#21691);
#6432=VERTEX_POINT('',#21717);
#6433=VERTEX_POINT('',#21728);
#6434=VERTEX_POINT('',#21890);
#6435=VERTEX_POINT('',#21891);
#6436=VERTEX_POINT('',#21898);
#6437=VERTEX_POINT('',#21909);
#6438=VERTEX_POINT('',#22398);
#6439=VERTEX_POINT('',#22482);
#6440=VERTEX_POINT('',#22579);
#6441=VERTEX_POINT('',#22601);
#6442=VERTEX_POINT('',#22603);
#6443=VERTEX_POINT('',#22607);
#6444=VERTEX_POINT('',#22610);
#6445=VERTEX_POINT('',#22614);
#6446=VERTEX_POINT('',#22617);
#6447=VERTEX_POINT('',#22628);
#6448=VERTEX_POINT('',#22630);
#6449=VERTEX_POINT('',#22632);
#6450=VERTEX_POINT('',#22636);
#6451=VERTEX_POINT('',#22639);
#6452=VERTEX_POINT('',#22643);
#6453=VERTEX_POINT('',#22645);
#6454=VERTEX_POINT('',#22649);
#6455=VERTEX_POINT('',#22650);
#6456=VERTEX_POINT('',#22652);
#6457=VERTEX_POINT('',#22654);
#6458=VERTEX_POINT('',#22656);
#6459=VERTEX_POINT('',#22658);
#6460=VERTEX_POINT('',#22660);
#6461=VERTEX_POINT('',#22662);
#6462=VERTEX_POINT('',#22666);
#6463=VERTEX_POINT('',#22668);
#6464=VERTEX_POINT('',#22704);
#6465=VERTEX_POINT('',#22738);
#6466=VERTEX_POINT('',#22740);
#6467=VERTEX_POINT('',#22742);
#6468=VERTEX_POINT('',#22793);
#6469=VERTEX_POINT('',#22794);
#6470=VERTEX_POINT('',#22796);
#6471=VERTEX_POINT('',#22809);
#6472=VERTEX_POINT('',#22848);
#6473=VERTEX_POINT('',#22849);
#6474=VERTEX_POINT('',#22851);
#6475=VERTEX_POINT('',#22853);
#6476=VERTEX_POINT('',#22912);
#6477=VERTEX_POINT('',#22913);
#6478=VERTEX_POINT('',#22915);
#6479=VERTEX_POINT('',#22924);
#6480=VERTEX_POINT('',#22983);
#6481=VERTEX_POINT('',#22987);
#6482=VERTEX_POINT('',#22992);
#6483=VERTEX_POINT('',#22999);
#6484=VERTEX_POINT('',#23004);
#6485=VERTEX_POINT('',#23006);
#6486=VERTEX_POINT('',#23008);
#6487=VERTEX_POINT('',#23012);
#6488=VERTEX_POINT('',#23016);
#6489=VERTEX_POINT('',#23018);
#6490=VERTEX_POINT('',#23069);
#6491=VERTEX_POINT('',#23070);
#6492=VERTEX_POINT('',#23072);
#6493=VERTEX_POINT('',#23085);
#6494=VERTEX_POINT('',#23087);
#6495=VERTEX_POINT('',#23129);
#6496=VERTEX_POINT('',#23130);
#6497=VERTEX_POINT('',#23132);
#6498=VERTEX_POINT('',#23134);
#6499=VERTEX_POINT('',#23193);
#6500=VERTEX_POINT('',#23194);
#6501=VERTEX_POINT('',#23196);
#6502=VERTEX_POINT('',#23205);
#6503=VERTEX_POINT('',#23264);
#6504=VERTEX_POINT('',#23268);
#6505=VERTEX_POINT('',#23270);
#6506=VERTEX_POINT('',#23274);
#6507=VERTEX_POINT('',#23278);
#6508=VERTEX_POINT('',#23280);
#6509=VERTEX_POINT('',#23282);
#6510=VERTEX_POINT('',#23325);
#6511=VERTEX_POINT('',#23326);
#6512=VERTEX_POINT('',#23328);
#6513=VERTEX_POINT('',#23339);
#6514=VERTEX_POINT('',#23376);
#6515=VERTEX_POINT('',#23378);
#6516=VERTEX_POINT('',#23380);
#6517=VERTEX_POINT('',#23431);
#6518=VERTEX_POINT('',#23433);
#6519=VERTEX_POINT('',#23482);
#6520=VERTEX_POINT('',#23486);
#6521=VERTEX_POINT('',#23488);
#6522=VERTEX_POINT('',#23515);
#6523=VERTEX_POINT('',#23516);
#6524=VERTEX_POINT('',#23518);
#6525=VERTEX_POINT('',#23525);
#6526=VERTEX_POINT('',#23558);
#6527=VERTEX_POINT('',#23559);
#6528=VERTEX_POINT('',#23561);
#6529=VERTEX_POINT('',#23563);
#6530=VERTEX_POINT('',#23642);
#6531=VERTEX_POINT('',#23643);
#6532=VERTEX_POINT('',#23645);
#6533=VERTEX_POINT('',#23659);
#6534=VERTEX_POINT('',#23661);
#6535=VERTEX_POINT('',#23728);
#6536=VERTEX_POINT('',#23732);
#6537=VERTEX_POINT('',#23734);
#6538=VERTEX_POINT('',#23738);
#6539=VERTEX_POINT('',#23757);
#6540=VERTEX_POINT('',#23758);
#6541=VERTEX_POINT('',#23763);
#6542=VERTEX_POINT('',#23768);
#6543=VERTEX_POINT('',#23817);
#6544=VERTEX_POINT('',#23831);
#6545=VERTEX_POINT('',#23859);
#6546=VERTEX_POINT('',#23864);
#6547=VERTEX_POINT('',#23869);
#6548=VERTEX_POINT('',#23879);
#6549=VERTEX_POINT('',#23880);
#6550=VERTEX_POINT('',#23893);
#6551=VERTEX_POINT('',#23895);
#6552=VERTEX_POINT('',#23938);
#6553=VERTEX_POINT('',#23948);
#6554=VERTEX_POINT('',#23959);
#6555=VERTEX_POINT('',#23961);
#6556=VERTEX_POINT('',#23978);
#6557=VERTEX_POINT('',#24001);
#6558=VERTEX_POINT('',#24002);
#6559=VERTEX_POINT('',#24007);
#6560=VERTEX_POINT('',#24013);
#6561=VERTEX_POINT('',#24018);
#6562=VERTEX_POINT('',#24044);
#6563=VERTEX_POINT('',#24051);
#6564=VERTEX_POINT('',#24110);
#6565=VERTEX_POINT('',#24123);
#6566=VERTEX_POINT('',#24138);
#6567=VERTEX_POINT('',#24139);
#6568=VERTEX_POINT('',#24141);
#6569=VERTEX_POINT('',#24143);
#6570=VERTEX_POINT('',#24197);
#6571=VERTEX_POINT('',#24207);
#6572=VERTEX_POINT('',#24209);
#6573=VERTEX_POINT('',#24213);
#6574=VERTEX_POINT('',#24215);
#6575=VERTEX_POINT('',#24217);
#6576=VERTEX_POINT('',#24219);
#6577=VERTEX_POINT('',#24221);
#6578=VERTEX_POINT('',#24223);
#6579=VERTEX_POINT('',#24225);
#6580=VERTEX_POINT('',#24227);
#6581=VERTEX_POINT('',#24229);
#6582=VERTEX_POINT('',#24231);
#6583=VERTEX_POINT('',#24233);
#6584=VERTEX_POINT('',#24235);
#6585=VERTEX_POINT('',#24237);
#6586=VERTEX_POINT('',#24243);
#6587=VERTEX_POINT('',#24245);
#6588=VERTEX_POINT('',#24249);
#6589=VERTEX_POINT('',#24250);
#6590=VERTEX_POINT('',#24252);
#6591=VERTEX_POINT('',#24254);
#6592=VERTEX_POINT('',#24257);
#6593=VERTEX_POINT('',#24259);
#6594=VERTEX_POINT('',#24261);
#6595=VERTEX_POINT('',#24263);
#6596=VERTEX_POINT('',#24266);
#6597=VERTEX_POINT('',#24270);
#6598=VERTEX_POINT('',#24274);
#6599=VERTEX_POINT('',#24278);
#6600=VERTEX_POINT('',#24282);
#6601=VERTEX_POINT('',#24286);
#6602=VERTEX_POINT('',#24290);
#6603=VERTEX_POINT('',#24294);
#6604=VERTEX_POINT('',#24298);
#6605=VERTEX_POINT('',#24300);
#6606=VERTEX_POINT('',#24316);
#6607=VERTEX_POINT('',#24443);
#6608=VERTEX_POINT('',#24468);
#6609=VERTEX_POINT('',#24472);
#6610=VERTEX_POINT('',#24473);
#6611=VERTEX_POINT('',#24475);
#6612=VERTEX_POINT('',#24477);
#6613=VERTEX_POINT('',#24494);
#6614=VERTEX_POINT('',#24496);
#6615=VERTEX_POINT('',#24503);
#6616=VERTEX_POINT('',#24504);
#6617=VERTEX_POINT('',#24522);
#6618=VERTEX_POINT('',#24529);
#6619=VERTEX_POINT('',#24548);
#6620=VERTEX_POINT('',#24550);
#6621=VERTEX_POINT('',#24560);
#6622=VERTEX_POINT('',#24564);
#6623=VERTEX_POINT('',#24565);
#6624=VERTEX_POINT('',#24583);
#6625=VERTEX_POINT('',#24592);
#6626=VERTEX_POINT('',#24593);
#6627=VERTEX_POINT('',#24616);
#6628=VERTEX_POINT('',#24618);
#6629=VERTEX_POINT('',#24621);
#6630=VERTEX_POINT('',#24623);
#6631=VERTEX_POINT('',#24626);
#6632=VERTEX_POINT('',#24628);
#6633=VERTEX_POINT('',#24630);
#6634=VERTEX_POINT('',#24632);
#6635=VERTEX_POINT('',#24634);
#6636=VERTEX_POINT('',#24637);
#6637=VERTEX_POINT('',#24639);
#6638=VERTEX_POINT('',#24643);
#6639=VERTEX_POINT('',#24647);
#6640=VERTEX_POINT('',#24651);
#6641=VERTEX_POINT('',#24764);
#6642=VERTEX_POINT('',#24766);
#6643=VERTEX_POINT('',#25078);
#6644=VERTEX_POINT('',#25081);
#6645=VERTEX_POINT('',#25083);
#6646=VERTEX_POINT('',#25100);
#6647=VERTEX_POINT('',#25103);
#6648=VERTEX_POINT('',#25106);
#6649=VERTEX_POINT('',#25107);
#6650=VERTEX_POINT('',#25128);
#6651=VERTEX_POINT('',#25130);
#6652=VERTEX_POINT('',#25147);
#6653=VERTEX_POINT('',#25149);
#6654=VERTEX_POINT('',#25151);
#6655=VERTEX_POINT('',#25156);
#6656=VERTEX_POINT('',#25157);
#6657=VERTEX_POINT('',#25172);
#6658=VERTEX_POINT('',#25174);
#6659=VERTEX_POINT('',#25191);
#6660=VERTEX_POINT('',#25193);
#6661=VERTEX_POINT('',#25196);
#6662=VERTEX_POINT('',#25199);
#6663=VERTEX_POINT('',#25200);
#6664=VERTEX_POINT('',#25215);
#6665=VERTEX_POINT('',#25217);
#6666=VERTEX_POINT('',#25234);
#6667=VERTEX_POINT('',#25236);
#6668=VERTEX_POINT('',#25239);
#6669=VERTEX_POINT('',#25242);
#6670=VERTEX_POINT('',#25250);
#6671=VERTEX_POINT('',#25254);
#6672=VERTEX_POINT('',#25256);
#6673=VERTEX_POINT('',#25262);
#6674=VERTEX_POINT('',#25264);
#6675=VERTEX_POINT('',#25268);
#6676=VERTEX_POINT('',#25272);
#6677=VERTEX_POINT('',#25276);
#6678=VERTEX_POINT('',#25280);
#6679=VERTEX_POINT('',#25284);
#6680=VERTEX_POINT('',#25291);
#6681=VERTEX_POINT('',#25300);
#6682=VERTEX_POINT('',#25336);
#6683=VERTEX_POINT('',#25340);
#6684=VERTEX_POINT('',#25344);
#6685=VERTEX_POINT('',#25349);
#6686=VERTEX_POINT('',#25380);
#6687=VERTEX_POINT('',#25401);
#6688=VERTEX_POINT('',#25405);
#6689=VERTEX_POINT('',#25413);
#6690=VERTEX_POINT('',#25414);
#6691=VERTEX_POINT('',#25416);
#6692=VERTEX_POINT('',#25418);
#6693=VERTEX_POINT('',#25422);
#6694=VERTEX_POINT('',#25424);
#6695=VERTEX_POINT('',#25428);
#6696=VERTEX_POINT('',#25430);
#6697=VERTEX_POINT('',#25432);
#6698=VERTEX_POINT('',#25434);
#6699=VERTEX_POINT('',#25436);
#6700=VERTEX_POINT('',#25440);
#6701=VERTEX_POINT('',#25444);
#6702=VERTEX_POINT('',#25447);
#6703=VERTEX_POINT('',#25450);
#6704=VERTEX_POINT('',#25451);
#6705=VERTEX_POINT('',#25457);
#6706=VERTEX_POINT('',#25460);
#6707=VERTEX_POINT('',#25470);
#6708=VERTEX_POINT('',#25471);
#6709=VERTEX_POINT('',#25474);
#6710=VERTEX_POINT('',#25478);
#6711=VERTEX_POINT('',#25480);
#6712=VERTEX_POINT('',#25482);
#6713=VERTEX_POINT('',#25484);
#6714=VERTEX_POINT('',#25486);
#6715=VERTEX_POINT('',#25488);
#6716=VERTEX_POINT('',#25490);
#6717=VERTEX_POINT('',#25492);
#6718=VERTEX_POINT('',#25493);
#6719=VERTEX_POINT('',#25495);
#6720=VERTEX_POINT('',#25497);
#6721=VERTEX_POINT('',#25501);
#6722=VERTEX_POINT('',#25505);
#6723=VERTEX_POINT('',#25506);
#6724=VERTEX_POINT('',#25511);
#6725=VERTEX_POINT('',#25513);
#6726=VERTEX_POINT('',#25519);
#6727=VERTEX_POINT('',#25521);
#6728=VERTEX_POINT('',#25525);
#6729=VERTEX_POINT('',#25529);
#6730=VERTEX_POINT('',#25531);
#6731=VERTEX_POINT('',#25533);
#6732=VERTEX_POINT('',#25539);
#6733=VERTEX_POINT('',#25543);
#6734=VERTEX_POINT('',#25549);
#6735=VERTEX_POINT('',#25551);
#6736=VERTEX_POINT('',#25553);
#6737=VERTEX_POINT('',#25555);
#6738=VERTEX_POINT('',#25557);
#6739=VERTEX_POINT('',#25559);
#6740=VERTEX_POINT('',#25561);
#6741=VERTEX_POINT('',#25563);
#6742=VERTEX_POINT('',#25566);
#6743=VERTEX_POINT('',#25570);
#6744=VERTEX_POINT('',#25575);
#6745=VERTEX_POINT('',#25579);
#6746=VERTEX_POINT('',#25584);
#6747=VERTEX_POINT('',#25588);
#6748=VERTEX_POINT('',#25593);
#6749=VERTEX_POINT('',#25597);
#6750=VERTEX_POINT('',#25602);
#6751=VERTEX_POINT('',#25606);
#6752=VERTEX_POINT('',#25611);
#6753=VERTEX_POINT('',#25615);
#6754=VERTEX_POINT('',#25620);
#6755=VERTEX_POINT('',#25624);
#6756=VERTEX_POINT('',#25632);
#6757=VERTEX_POINT('',#25633);
#6758=VERTEX_POINT('',#25635);
#6759=VERTEX_POINT('',#25637);
#6760=VERTEX_POINT('',#25641);
#6761=VERTEX_POINT('',#25643);
#6762=VERTEX_POINT('',#25647);
#6763=VERTEX_POINT('',#25649);
#6764=VERTEX_POINT('',#25653);
#6765=VERTEX_POINT('',#25654);
#6766=VERTEX_POINT('',#25656);
#6767=VERTEX_POINT('',#25658);
#6768=VERTEX_POINT('',#25662);
#6769=VERTEX_POINT('',#25664);
#6770=VERTEX_POINT('',#25668);
#6771=VERTEX_POINT('',#25670);
#6772=VERTEX_POINT('',#25674);
#6773=VERTEX_POINT('',#25675);
#6774=VERTEX_POINT('',#25677);
#6775=VERTEX_POINT('',#25679);
#6776=VERTEX_POINT('',#25683);
#6777=VERTEX_POINT('',#25685);
#6778=VERTEX_POINT('',#25689);
#6779=VERTEX_POINT('',#25691);
#6780=VERTEX_POINT('',#25695);
#6781=VERTEX_POINT('',#25696);
#6782=VERTEX_POINT('',#25698);
#6783=VERTEX_POINT('',#25700);
#6784=VERTEX_POINT('',#25704);
#6785=VERTEX_POINT('',#25706);
#6786=VERTEX_POINT('',#25710);
#6787=VERTEX_POINT('',#25712);
#6788=VERTEX_POINT('',#25728);
#6789=VERTEX_POINT('',#25730);
#6790=VERTEX_POINT('',#25734);
#6791=VERTEX_POINT('',#25737);
#6792=VERTEX_POINT('',#25743);
#6793=VERTEX_POINT('',#25744);
#6794=VERTEX_POINT('',#25746);
#6795=VERTEX_POINT('',#25750);
#6796=VERTEX_POINT('',#25757);
#6797=VERTEX_POINT('',#25758);
#6798=VERTEX_POINT('',#25760);
#6799=VERTEX_POINT('',#25764);
#6800=VERTEX_POINT('',#25772);
#6801=VERTEX_POINT('',#25776);
#6802=VERTEX_POINT('',#25782);
#6803=VERTEX_POINT('',#25784);
#6804=VERTEX_POINT('',#25786);
#6805=VERTEX_POINT('',#25788);
#6806=VERTEX_POINT('',#25794);
#6807=VERTEX_POINT('',#25798);
#6808=VERTEX_POINT('',#25802);
#6809=VERTEX_POINT('',#25804);
#6810=VERTEX_POINT('',#25808);
#6811=VERTEX_POINT('',#25809);
#6812=VERTEX_POINT('',#25811);
#6813=VERTEX_POINT('',#25815);
#6814=VERTEX_POINT('',#25822);
#6815=VERTEX_POINT('',#25823);
#6816=VERTEX_POINT('',#25825);
#6817=VERTEX_POINT('',#25829);
#6818=VERTEX_POINT('',#25837);
#6819=VERTEX_POINT('',#25841);
#6820=VERTEX_POINT('',#25847);
#6821=VERTEX_POINT('',#25849);
#6822=VERTEX_POINT('',#25851);
#6823=VERTEX_POINT('',#25853);
#6824=VERTEX_POINT('',#25859);
#6825=VERTEX_POINT('',#25863);
#6826=VERTEX_POINT('',#25867);
#6827=VERTEX_POINT('',#25869);
#6828=VERTEX_POINT('',#25873);
#6829=VERTEX_POINT('',#25874);
#6830=VERTEX_POINT('',#25876);
#6831=VERTEX_POINT('',#25880);
#6832=VERTEX_POINT('',#25887);
#6833=VERTEX_POINT('',#25888);
#6834=VERTEX_POINT('',#25890);
#6835=VERTEX_POINT('',#25894);
#6836=VERTEX_POINT('',#25902);
#6837=VERTEX_POINT('',#25906);
#6838=VERTEX_POINT('',#25912);
#6839=VERTEX_POINT('',#25914);
#6840=VERTEX_POINT('',#25916);
#6841=VERTEX_POINT('',#25918);
#6842=VERTEX_POINT('',#25924);
#6843=VERTEX_POINT('',#25928);
#6844=VERTEX_POINT('',#25932);
#6845=VERTEX_POINT('',#25934);
#6846=VERTEX_POINT('',#25938);
#6847=VERTEX_POINT('',#25939);
#6848=VERTEX_POINT('',#25941);
#6849=VERTEX_POINT('',#25945);
#6850=VERTEX_POINT('',#25952);
#6851=VERTEX_POINT('',#25953);
#6852=VERTEX_POINT('',#25955);
#6853=VERTEX_POINT('',#25959);
#6854=VERTEX_POINT('',#25967);
#6855=VERTEX_POINT('',#25971);
#6856=VERTEX_POINT('',#25977);
#6857=VERTEX_POINT('',#25979);
#6858=VERTEX_POINT('',#25981);
#6859=VERTEX_POINT('',#25983);
#6860=VERTEX_POINT('',#25989);
#6861=VERTEX_POINT('',#25993);
#6862=VERTEX_POINT('',#25997);
#6863=VERTEX_POINT('',#25999);
#6864=VERTEX_POINT('',#26003);
#6865=VERTEX_POINT('',#26004);
#6866=VERTEX_POINT('',#26008);
#6867=VERTEX_POINT('',#26010);
#6868=VERTEX_POINT('',#26016);
#6869=VERTEX_POINT('',#26020);
#6870=VERTEX_POINT('',#26022);
#6871=VERTEX_POINT('',#26024);
#6872=VERTEX_POINT('',#26026);
#6873=VERTEX_POINT('',#26032);
#6874=VERTEX_POINT('',#26033);
#6875=VERTEX_POINT('',#26035);
#6876=VERTEX_POINT('',#26039);
#6877=VERTEX_POINT('',#26046);
#6878=VERTEX_POINT('',#26053);
#6879=VERTEX_POINT('',#26057);
#6880=VERTEX_POINT('',#26059);
#6881=VERTEX_POINT('',#26061);
#6882=VERTEX_POINT('',#26065);
#6883=VERTEX_POINT('',#26067);
#6884=VERTEX_POINT('',#26071);
#6885=VERTEX_POINT('',#26077);
#6886=VERTEX_POINT('',#26079);
#6887=VERTEX_POINT('',#26081);
#6888=VERTEX_POINT('',#26083);
#6889=VERTEX_POINT('',#26085);
#6890=VERTEX_POINT('',#26087);
#6891=VERTEX_POINT('',#26089);
#6892=VERTEX_POINT('',#26091);
#6893=VERTEX_POINT('',#26093);
#6894=VERTEX_POINT('',#26095);
#6895=VERTEX_POINT('',#26097);
#6896=VERTEX_POINT('',#26099);
#6897=VERTEX_POINT('',#26101);
#6898=VERTEX_POINT('',#26103);
#6899=VERTEX_POINT('',#26105);
#6900=VERTEX_POINT('',#26112);
#6901=VERTEX_POINT('',#26114);
#6902=VERTEX_POINT('',#26116);
#6903=VERTEX_POINT('',#26118);
#6904=VERTEX_POINT('',#26120);
#6905=VERTEX_POINT('',#26122);
#6906=VERTEX_POINT('',#26124);
#6907=VERTEX_POINT('',#26126);
#6908=VERTEX_POINT('',#26128);
#6909=VERTEX_POINT('',#26130);
#6910=VERTEX_POINT('',#26132);
#6911=VERTEX_POINT('',#26134);
#6912=VERTEX_POINT('',#26136);
#6913=VERTEX_POINT('',#26138);
#6914=VERTEX_POINT('',#26140);
#6915=VERTEX_POINT('',#26142);
#6916=VERTEX_POINT('',#26144);
#6917=VERTEX_POINT('',#26146);
#6918=VERTEX_POINT('',#26150);
#6919=VERTEX_POINT('',#26157);
#6920=VERTEX_POINT('',#26161);
#6921=VERTEX_POINT('',#26168);
#6922=VERTEX_POINT('',#26172);
#6923=VERTEX_POINT('',#26178);
#6924=VERTEX_POINT('',#26180);
#6925=VERTEX_POINT('',#26182);
#6926=VERTEX_POINT('',#26186);
#6927=VERTEX_POINT('',#26190);
#6928=VERTEX_POINT('',#26194);
#6929=VERTEX_POINT('',#26196);
#6930=VERTEX_POINT('',#26200);
#6931=VERTEX_POINT('',#26201);
#6932=VERTEX_POINT('',#26211);
#6933=VERTEX_POINT('',#26215);
#6934=VERTEX_POINT('',#26222);
#6935=VERTEX_POINT('',#26226);
#6936=VERTEX_POINT('',#26232);
#6937=VERTEX_POINT('',#26234);
#6938=VERTEX_POINT('',#26236);
#6939=VERTEX_POINT('',#26238);
#6940=VERTEX_POINT('',#26244);
#6941=VERTEX_POINT('',#26248);
#6942=VERTEX_POINT('',#26252);
#6943=VERTEX_POINT('',#26254);
#6944=VERTEX_POINT('',#26258);
#6945=VERTEX_POINT('',#26259);
#6946=VERTEX_POINT('',#26261);
#6947=VERTEX_POINT('',#26263);
#6948=VERTEX_POINT('',#26267);
#6949=VERTEX_POINT('',#26269);
#6950=VERTEX_POINT('',#26273);
#6951=VERTEX_POINT('',#26274);
#6952=VERTEX_POINT('',#26276);
#6953=VERTEX_POINT('',#26278);
#6954=VERTEX_POINT('',#26282);
#6955=VERTEX_POINT('',#26284);
#6956=VERTEX_POINT('',#26288);
#6957=VERTEX_POINT('',#26289);
#6958=VERTEX_POINT('',#26291);
#6959=VERTEX_POINT('',#26293);
#6960=VERTEX_POINT('',#26297);
#6961=VERTEX_POINT('',#26299);
#6962=VERTEX_POINT('',#26303);
#6963=VERTEX_POINT('',#26304);
#6964=VERTEX_POINT('',#26306);
#6965=VERTEX_POINT('',#26308);
#6966=VERTEX_POINT('',#26312);
#6967=VERTEX_POINT('',#26314);
#6968=VERTEX_POINT('',#26318);
#6969=VERTEX_POINT('',#26319);
#6970=VERTEX_POINT('',#26321);
#6971=VERTEX_POINT('',#26323);
#6972=VERTEX_POINT('',#26327);
#6973=VERTEX_POINT('',#26329);
#6974=VERTEX_POINT('',#26362);
#6975=VERTEX_POINT('',#26363);
#6976=VERTEX_POINT('',#26373);
#6977=VERTEX_POINT('',#26377);
#6978=VERTEX_POINT('',#26384);
#6979=VERTEX_POINT('',#26388);
#6980=VERTEX_POINT('',#26395);
#6981=VERTEX_POINT('',#26403);
#6982=VERTEX_POINT('',#26409);
#6983=VERTEX_POINT('',#26410);
#6984=VERTEX_POINT('',#26420);
#6985=VERTEX_POINT('',#26424);
#6986=VERTEX_POINT('',#26431);
#6987=VERTEX_POINT('',#26435);
#6988=VERTEX_POINT('',#26442);
#6989=VERTEX_POINT('',#26450);
#6990=VERTEX_POINT('',#26456);
#6991=VERTEX_POINT('',#26457);
#6992=VERTEX_POINT('',#26467);
#6993=VERTEX_POINT('',#26471);
#6994=VERTEX_POINT('',#26478);
#6995=VERTEX_POINT('',#26482);
#6996=VERTEX_POINT('',#26489);
#6997=VERTEX_POINT('',#26497);
#6998=VERTEX_POINT('',#26503);
#6999=VERTEX_POINT('',#26504);
#7000=VERTEX_POINT('',#26514);
#7001=VERTEX_POINT('',#26518);
#7002=VERTEX_POINT('',#26525);
#7003=VERTEX_POINT('',#26529);
#7004=VERTEX_POINT('',#26536);
#7005=VERTEX_POINT('',#26544);
#7006=VERTEX_POINT('',#26550);
#7007=VERTEX_POINT('',#26551);
#7008=VERTEX_POINT('',#26561);
#7009=VERTEX_POINT('',#26565);
#7010=VERTEX_POINT('',#26572);
#7011=VERTEX_POINT('',#26576);
#7012=VERTEX_POINT('',#26585);
#7013=VERTEX_POINT('',#26591);
#7014=VERTEX_POINT('',#26595);
#7015=VERTEX_POINT('',#26601);
#7016=VERTEX_POINT('',#26602);
#7017=VERTEX_POINT('',#26604);
#7018=VERTEX_POINT('',#26606);
#7019=VERTEX_POINT('',#26610);
#7020=VERTEX_POINT('',#26612);
#7021=VERTEX_POINT('',#26616);
#7022=VERTEX_POINT('',#26623);
#7023=VERTEX_POINT('',#26627);
#7024=VERTEX_POINT('',#26634);
#7025=VERTEX_POINT('',#26638);
#7026=VERTEX_POINT('',#26647);
#7027=VERTEX_POINT('',#26655);
#7028=VERTEX_POINT('',#26657);
#7029=VERTEX_POINT('',#26661);
#7030=VERTEX_POINT('',#26675);
#7031=VERTEX_POINT('',#26680);
#7032=VERTEX_POINT('',#26681);
#7033=VERTEX_POINT('',#26683);
#7034=VERTEX_POINT('',#26685);
#7035=VERTEX_POINT('',#26689);
#7036=VERTEX_POINT('',#26691);
#7037=VERTEX_POINT('',#26695);
#7038=VERTEX_POINT('',#26697);
#7039=VERTEX_POINT('',#26721);
#7040=VERTEX_POINT('',#26724);
#7041=VERTEX_POINT('',#26728);
#7042=VERTEX_POINT('',#26731);
#7043=VERTEX_POINT('',#26735);
#7044=VERTEX_POINT('',#26738);
#7045=VERTEX_POINT('',#26742);
#7046=VERTEX_POINT('',#26748);
#7047=VERTEX_POINT('',#26749);
#7048=VERTEX_POINT('',#26751);
#7049=VERTEX_POINT('',#26753);
#7050=VERTEX_POINT('',#26755);
#7051=VERTEX_POINT('',#26757);
#7052=VERTEX_POINT('',#26761);
#7053=VERTEX_POINT('',#26763);
#7054=VERTEX_POINT('',#26767);
#7055=VERTEX_POINT('',#26769);
#7056=VERTEX_POINT('',#26771);
#7057=VERTEX_POINT('',#26775);
#7058=VERTEX_POINT('',#26777);
#7059=VERTEX_POINT('',#26779);
#7060=VERTEX_POINT('',#26783);
#7061=VERTEX_POINT('',#26784);
#7062=VERTEX_POINT('',#26786);
#7063=VERTEX_POINT('',#26789);
#7064=VERTEX_POINT('',#26793);
#7065=VERTEX_POINT('',#26795);
#7066=VERTEX_POINT('',#26799);
#7067=VERTEX_POINT('',#26801);
#7068=VERTEX_POINT('',#26803);
#7069=VERTEX_POINT('',#26807);
#7070=VERTEX_POINT('',#26812);
#7071=VERTEX_POINT('',#26816);
#7072=VERTEX_POINT('',#26818);
#7073=VERTEX_POINT('',#26820);
#7074=VERTEX_POINT('',#26824);
#7075=VERTEX_POINT('',#26829);
#7076=VERTEX_POINT('',#26833);
#7077=VERTEX_POINT('',#26835);
#7078=VERTEX_POINT('',#26847);
#7079=VERTEX_POINT('',#26849);
#7080=VERTEX_POINT('',#26853);
#7081=VERTEX_POINT('',#26856);
#7082=VERTEX_POINT('',#26860);
#7083=VERTEX_POINT('',#26863);
#7084=VERTEX_POINT('',#26867);
#7085=VERTEX_POINT('',#26871);
#7086=VERTEX_POINT('',#26875);
#7087=VERTEX_POINT('',#26878);
#7088=VERTEX_POINT('',#26882);
#7089=VERTEX_POINT('',#26885);
#7090=VERTEX_POINT('',#26889);
#7091=VERTEX_POINT('',#26892);
#7092=VERTEX_POINT('',#26896);
#7093=VERTEX_POINT('',#26900);
#7094=VERTEX_POINT('',#26906);
#7095=VERTEX_POINT('',#26908);
#7096=VERTEX_POINT('',#26912);
#7097=VERTEX_POINT('',#26915);
#7098=VERTEX_POINT('',#26918);
#7099=VERTEX_POINT('',#26922);
#7100=VERTEX_POINT('',#26924);
#7101=VERTEX_POINT('',#26928);
#7102=VERTEX_POINT('',#26931);
#7103=VERTEX_POINT('',#26935);
#7104=VERTEX_POINT('',#26938);
#7105=VERTEX_POINT('',#26943);
#7106=VERTEX_POINT('',#26949);
#7107=VERTEX_POINT('',#26950);
#7108=VERTEX_POINT('',#26953);
#7109=VERTEX_POINT('',#26957);
#7110=VERTEX_POINT('',#26960);
#7111=VERTEX_POINT('',#26964);
#7112=VERTEX_POINT('',#26965);
#7113=VERTEX_POINT('',#26968);
#7114=VERTEX_POINT('',#26972);
#7115=VERTEX_POINT('',#26975);
#7116=VERTEX_POINT('',#26979);
#7117=VERTEX_POINT('',#26983);
#7118=VERTEX_POINT('',#26988);
#7119=VERTEX_POINT('',#26994);
#7120=VERTEX_POINT('',#26996);
#7121=VERTEX_POINT('',#27000);
#7122=VERTEX_POINT('',#27004);
#7123=VERTEX_POINT('',#27007);
#7124=VERTEX_POINT('',#27008);
#7125=VERTEX_POINT('',#27010);
#7126=VERTEX_POINT('',#27016);
#7127=VERTEX_POINT('',#27018);
#7128=VERTEX_POINT('',#27020);
#7129=VERTEX_POINT('',#27024);
#7130=VERTEX_POINT('',#27027);
#7131=VERTEX_POINT('',#27031);
#7132=VERTEX_POINT('',#27084);
#7133=VERTEX_POINT('',#27086);
#7134=VERTEX_POINT('',#27090);
#7135=VERTEX_POINT('',#27093);
#7136=VERTEX_POINT('',#27097);
#7137=VERTEX_POINT('',#27101);
#7138=VERTEX_POINT('',#27104);
#7139=VERTEX_POINT('',#27108);
#7140=VERTEX_POINT('',#27111);
#7141=VERTEX_POINT('',#27112);
#7142=VERTEX_POINT('',#27114);
#7143=VERTEX_POINT('',#27116);
#7144=VERTEX_POINT('',#27119);
#7145=VERTEX_POINT('',#27122);
#7146=VERTEX_POINT('',#27128);
#7147=VERTEX_POINT('',#27130);
#7148=VERTEX_POINT('',#27132);
#7149=VERTEX_POINT('',#27136);
#7150=VERTEX_POINT('',#27137);
#7151=VERTEX_POINT('',#27139);
#7152=VERTEX_POINT('',#27141);
#7153=VERTEX_POINT('',#27143);
#7154=VERTEX_POINT('',#27145);
#7155=VERTEX_POINT('',#27147);
#7156=VERTEX_POINT('',#27149);
#7157=VERTEX_POINT('',#27151);
#7158=VERTEX_POINT('',#27153);
#7159=VERTEX_POINT('',#27155);
#7160=VERTEX_POINT('',#27157);
#7161=VERTEX_POINT('',#27159);
#7162=VERTEX_POINT('',#27161);
#7163=VERTEX_POINT('',#27165);
#7164=VERTEX_POINT('',#27169);
#7165=VERTEX_POINT('',#27170);
#7166=VERTEX_POINT('',#27175);
#7167=VERTEX_POINT('',#27179);
#7168=VERTEX_POINT('',#27183);
#7169=VERTEX_POINT('',#27187);
#7170=VERTEX_POINT('',#27191);
#7171=VERTEX_POINT('',#27195);
#7172=VERTEX_POINT('',#27199);
#7173=VERTEX_POINT('',#27203);
#7174=VERTEX_POINT('',#27207);
#7175=VERTEX_POINT('',#27211);
#7176=VERTEX_POINT('',#27215);
#7177=VERTEX_POINT('',#27219);
#7178=VERTEX_POINT('',#27223);
#7179=VERTEX_POINT('',#27231);
#7180=VERTEX_POINT('',#27232);
#7181=VERTEX_POINT('',#27234);
#7182=VERTEX_POINT('',#27251);
#7183=VERTEX_POINT('',#27264);
#7184=VERTEX_POINT('',#27265);
#7185=VERTEX_POINT('',#27348);
#7186=VERTEX_POINT('',#27349);
#7187=VERTEX_POINT('',#27438);
#7188=VERTEX_POINT('',#27439);
#7189=VERTEX_POINT('',#27522);
#7190=VERTEX_POINT('',#27523);
#7191=VERTEX_POINT('',#27612);
#7192=VERTEX_POINT('',#27613);
#7193=VERTEX_POINT('',#27702);
#7194=VERTEX_POINT('',#27703);
#7195=VERTEX_POINT('',#27786);
#7196=VERTEX_POINT('',#27787);
#7197=VERTEX_POINT('',#27876);
#7198=VERTEX_POINT('',#27877);
#7199=VERTEX_POINT('',#27960);
#7200=VERTEX_POINT('',#27961);
#7201=VERTEX_POINT('',#28050);
#7202=VERTEX_POINT('',#28051);
#7203=VERTEX_POINT('',#28134);
#7204=VERTEX_POINT('',#28135);
#7205=VERTEX_POINT('',#28224);
#7206=VERTEX_POINT('',#28225);
#7207=VERTEX_POINT('',#28311);
#7208=VERTEX_POINT('',#28312);
#7209=VERTEX_POINT('',#28398);
#7210=VERTEX_POINT('',#28399);
#7211=VERTEX_POINT('',#28488);
#7212=VERTEX_POINT('',#28489);
#7213=VERTEX_POINT('',#28572);
#7214=VERTEX_POINT('',#28573);
#7215=VERTEX_POINT('',#28662);
#7216=VERTEX_POINT('',#28663);
#7217=VERTEX_POINT('',#28746);
#7218=VERTEX_POINT('',#28747);
#7219=VERTEX_POINT('',#28836);
#7220=VERTEX_POINT('',#28837);
#7221=VERTEX_POINT('',#28920);
#7222=VERTEX_POINT('',#28921);
#7223=VERTEX_POINT('',#29007);
#7224=VERTEX_POINT('',#29008);
#7225=VERTEX_POINT('',#29097);
#7226=VERTEX_POINT('',#29098);
#7227=VERTEX_POINT('',#29181);
#7228=VERTEX_POINT('',#29182);
#7229=VERTEX_POINT('',#29271);
#7230=VERTEX_POINT('',#29272);
#7231=VERTEX_POINT('',#29355);
#7232=VERTEX_POINT('',#29356);
#7233=VERTEX_POINT('',#29445);
#7234=VERTEX_POINT('',#29446);
#7235=VERTEX_POINT('',#29529);
#7236=VERTEX_POINT('',#29530);
#7237=VERTEX_POINT('',#29619);
#7238=VERTEX_POINT('',#29620);
#7239=VERTEX_POINT('',#29709);
#7240=VERTEX_POINT('',#29710);
#7241=VERTEX_POINT('',#29793);
#7242=VERTEX_POINT('',#29794);
#7243=VERTEX_POINT('',#29883);
#7244=VERTEX_POINT('',#29884);
#7245=VERTEX_POINT('',#29967);
#7246=VERTEX_POINT('',#29968);
#7247=VERTEX_POINT('',#30057);
#7248=VERTEX_POINT('',#30058);
#7249=VERTEX_POINT('',#30141);
#7250=VERTEX_POINT('',#30142);
#7251=VERTEX_POINT('',#30144);
#7252=VERTEX_POINT('',#30154);
#7253=VERTEX_POINT('',#30163);
#7254=VERTEX_POINT('',#30164);
#7255=VERTEX_POINT('',#30200);
#7256=VERTEX_POINT('',#30201);
#7257=VERTEX_POINT('',#30237);
#7258=VERTEX_POINT('',#30238);
#7259=VERTEX_POINT('',#30274);
#7260=VERTEX_POINT('',#30275);
#7261=VERTEX_POINT('',#30311);
#7262=VERTEX_POINT('',#30312);
#7263=VERTEX_POINT('',#30348);
#7264=VERTEX_POINT('',#30349);
#7265=VERTEX_POINT('',#30385);
#7266=VERTEX_POINT('',#30386);
#7267=VERTEX_POINT('',#30423);
#7268=VERTEX_POINT('',#30424);
#7269=VERTEX_POINT('',#30460);
#7270=VERTEX_POINT('',#30461);
#7271=VERTEX_POINT('',#30497);
#7272=VERTEX_POINT('',#30498);
#7273=VERTEX_POINT('',#30534);
#7274=VERTEX_POINT('',#30535);
#7275=VERTEX_POINT('',#30571);
#7276=VERTEX_POINT('',#30572);
#7277=VERTEX_POINT('',#30608);
#7278=VERTEX_POINT('',#30609);
#7279=VERTEX_POINT('',#30645);
#7280=VERTEX_POINT('',#30646);
#7281=VERTEX_POINT('',#30683);
#7282=VERTEX_POINT('',#30684);
#7283=VERTEX_POINT('',#30719);
#7284=VERTEX_POINT('',#30720);
#7285=VERTEX_POINT('',#30757);
#7286=VERTEX_POINT('',#30758);
#7287=VERTEX_POINT('',#30794);
#7288=VERTEX_POINT('',#30795);
#7289=VERTEX_POINT('',#30831);
#7290=VERTEX_POINT('',#30832);
#7291=VERTEX_POINT('',#30868);
#7292=VERTEX_POINT('',#30869);
#7293=VERTEX_POINT('',#30905);
#7294=VERTEX_POINT('',#30906);
#7295=VERTEX_POINT('',#30943);
#7296=VERTEX_POINT('',#30944);
#7297=VERTEX_POINT('',#30979);
#7298=VERTEX_POINT('',#30980);
#7299=VERTEX_POINT('',#31017);
#7300=VERTEX_POINT('',#31018);
#7301=VERTEX_POINT('',#31054);
#7302=VERTEX_POINT('',#31055);
#7303=VERTEX_POINT('',#31091);
#7304=VERTEX_POINT('',#31092);
#7305=VERTEX_POINT('',#31128);
#7306=VERTEX_POINT('',#31129);
#7307=VERTEX_POINT('',#31165);
#7308=VERTEX_POINT('',#31166);
#7309=VERTEX_POINT('',#31202);
#7310=VERTEX_POINT('',#31203);
#7311=VERTEX_POINT('',#31239);
#7312=VERTEX_POINT('',#31240);
#7313=VERTEX_POINT('',#31277);
#7314=VERTEX_POINT('',#31278);
#7315=VERTEX_POINT('',#31314);
#7316=VERTEX_POINT('',#31315);
#7317=VERTEX_POINT('',#31351);
#7318=VERTEX_POINT('',#31352);
#7319=VERTEX_POINT('',#33127);
#7320=VERTEX_POINT('',#33274);
#7321=VERTEX_POINT('',#33402);
#7322=VERTEX_POINT('',#33405);
#7323=VERTEX_POINT('',#35269);
#7324=VERTEX_POINT('',#35414);
#7325=VERTEX_POINT('',#35415);
#7326=VERTEX_POINT('',#35417);
#7327=VERTEX_POINT('',#35419);
#7328=VERTEX_POINT('',#35423);
#7329=VERTEX_POINT('',#35427);
#7330=VERTEX_POINT('',#35433);
#7331=VERTEX_POINT('',#35434);
#7332=VERTEX_POINT('',#35436);
#7333=VERTEX_POINT('',#35438);
#7334=VERTEX_POINT('',#35442);
#7335=VERTEX_POINT('',#35446);
#7336=VERTEX_POINT('',#35452);
#7337=VERTEX_POINT('',#35453);
#7338=VERTEX_POINT('',#35455);
#7339=VERTEX_POINT('',#35457);
#7340=VERTEX_POINT('',#35461);
#7341=VERTEX_POINT('',#35465);
#7342=VERTEX_POINT('',#35471);
#7343=VERTEX_POINT('',#35472);
#7344=VERTEX_POINT('',#35474);
#7345=VERTEX_POINT('',#35476);
#7346=VERTEX_POINT('',#35480);
#7347=VERTEX_POINT('',#35484);
#7348=VERTEX_POINT('',#35490);
#7349=VERTEX_POINT('',#35491);
#7350=VERTEX_POINT('',#35493);
#7351=VERTEX_POINT('',#35495);
#7352=VERTEX_POINT('',#35499);
#7353=VERTEX_POINT('',#35503);
#7354=VERTEX_POINT('',#35509);
#7355=VERTEX_POINT('',#35510);
#7356=VERTEX_POINT('',#35512);
#7357=VERTEX_POINT('',#35514);
#7358=VERTEX_POINT('',#35518);
#7359=VERTEX_POINT('',#35522);
#7360=VERTEX_POINT('',#35528);
#7361=VERTEX_POINT('',#35529);
#7362=VERTEX_POINT('',#35531);
#7363=VERTEX_POINT('',#35533);
#7364=VERTEX_POINT('',#35537);
#7365=VERTEX_POINT('',#35541);
#7366=VERTEX_POINT('',#35547);
#7367=VERTEX_POINT('',#35548);
#7368=VERTEX_POINT('',#35550);
#7369=VERTEX_POINT('',#35552);
#7370=VERTEX_POINT('',#35556);
#7371=VERTEX_POINT('',#35560);
#7372=VERTEX_POINT('',#35566);
#7373=VERTEX_POINT('',#35567);
#7374=VERTEX_POINT('',#35569);
#7375=VERTEX_POINT('',#35571);
#7376=VERTEX_POINT('',#35575);
#7377=VERTEX_POINT('',#35579);
#7378=VERTEX_POINT('',#35585);
#7379=VERTEX_POINT('',#35586);
#7380=VERTEX_POINT('',#35588);
#7381=VERTEX_POINT('',#35590);
#7382=VERTEX_POINT('',#35594);
#7383=VERTEX_POINT('',#35598);
#7384=VERTEX_POINT('',#35604);
#7385=VERTEX_POINT('',#35605);
#7386=VERTEX_POINT('',#35607);
#7387=VERTEX_POINT('',#35609);
#7388=VERTEX_POINT('',#35613);
#7389=VERTEX_POINT('',#35617);
#7390=VERTEX_POINT('',#35623);
#7391=VERTEX_POINT('',#35624);
#7392=VERTEX_POINT('',#35626);
#7393=VERTEX_POINT('',#35628);
#7394=VERTEX_POINT('',#35632);
#7395=VERTEX_POINT('',#35636);
#7396=VERTEX_POINT('',#35642);
#7397=VERTEX_POINT('',#35643);
#7398=VERTEX_POINT('',#35645);
#7399=VERTEX_POINT('',#35647);
#7400=VERTEX_POINT('',#35651);
#7401=VERTEX_POINT('',#35655);
#7402=VERTEX_POINT('',#35661);
#7403=VERTEX_POINT('',#35662);
#7404=VERTEX_POINT('',#35664);
#7405=VERTEX_POINT('',#35666);
#7406=VERTEX_POINT('',#35670);
#7407=VERTEX_POINT('',#35674);
#7408=VERTEX_POINT('',#35680);
#7409=VERTEX_POINT('',#35681);
#7410=VERTEX_POINT('',#35683);
#7411=VERTEX_POINT('',#35685);
#7412=VERTEX_POINT('',#35689);
#7413=VERTEX_POINT('',#35693);
#7414=VERTEX_POINT('',#35699);
#7415=VERTEX_POINT('',#35700);
#7416=VERTEX_POINT('',#35702);
#7417=VERTEX_POINT('',#35704);
#7418=VERTEX_POINT('',#35708);
#7419=VERTEX_POINT('',#35712);
#7420=VERTEX_POINT('',#35718);
#7421=VERTEX_POINT('',#35719);
#7422=VERTEX_POINT('',#35721);
#7423=VERTEX_POINT('',#35723);
#7424=VERTEX_POINT('',#35727);
#7425=VERTEX_POINT('',#35731);
#7426=VERTEX_POINT('',#35737);
#7427=VERTEX_POINT('',#35738);
#7428=VERTEX_POINT('',#35740);
#7429=VERTEX_POINT('',#35742);
#7430=VERTEX_POINT('',#35746);
#7431=VERTEX_POINT('',#35748);
#7432=VERTEX_POINT('',#35752);
#7433=VERTEX_POINT('',#35756);
#7434=VERTEX_POINT('',#35760);
#7435=VERTEX_POINT('',#35761);
#7436=VERTEX_POINT('',#35763);
#7437=VERTEX_POINT('',#35765);
#7438=VERTEX_POINT('',#35769);
#7439=VERTEX_POINT('',#35773);
#7440=VERTEX_POINT('',#35779);
#7441=VERTEX_POINT('',#35780);
#7442=VERTEX_POINT('',#35782);
#7443=VERTEX_POINT('',#35784);
#7444=VERTEX_POINT('',#35788);
#7445=VERTEX_POINT('',#35792);
#7446=VERTEX_POINT('',#35798);
#7447=VERTEX_POINT('',#35799);
#7448=VERTEX_POINT('',#35801);
#7449=VERTEX_POINT('',#35803);
#7450=VERTEX_POINT('',#35807);
#7451=VERTEX_POINT('',#35811);
#7452=VERTEX_POINT('',#35817);
#7453=VERTEX_POINT('',#35818);
#7454=VERTEX_POINT('',#35820);
#7455=VERTEX_POINT('',#35822);
#7456=VERTEX_POINT('',#35826);
#7457=VERTEX_POINT('',#35830);
#7458=VERTEX_POINT('',#35836);
#7459=VERTEX_POINT('',#35837);
#7460=VERTEX_POINT('',#35839);
#7461=VERTEX_POINT('',#35841);
#7462=VERTEX_POINT('',#35845);
#7463=VERTEX_POINT('',#35849);
#7464=VERTEX_POINT('',#35855);
#7465=VERTEX_POINT('',#35856);
#7466=VERTEX_POINT('',#35858);
#7467=VERTEX_POINT('',#35860);
#7468=VERTEX_POINT('',#35864);
#7469=VERTEX_POINT('',#35868);
#7470=VERTEX_POINT('',#35874);
#7471=VERTEX_POINT('',#35875);
#7472=VERTEX_POINT('',#35877);
#7473=VERTEX_POINT('',#35879);
#7474=VERTEX_POINT('',#35883);
#7475=VERTEX_POINT('',#35887);
#7476=VERTEX_POINT('',#35893);
#7477=VERTEX_POINT('',#35894);
#7478=VERTEX_POINT('',#35896);
#7479=VERTEX_POINT('',#35898);
#7480=VERTEX_POINT('',#35902);
#7481=VERTEX_POINT('',#35906);
#7482=VERTEX_POINT('',#35912);
#7483=VERTEX_POINT('',#35913);
#7484=VERTEX_POINT('',#35915);
#7485=VERTEX_POINT('',#35917);
#7486=VERTEX_POINT('',#35921);
#7487=VERTEX_POINT('',#35925);
#7488=VERTEX_POINT('',#35931);
#7489=VERTEX_POINT('',#35932);
#7490=VERTEX_POINT('',#35934);
#7491=VERTEX_POINT('',#35936);
#7492=VERTEX_POINT('',#35940);
#7493=VERTEX_POINT('',#35944);
#7494=VERTEX_POINT('',#35950);
#7495=VERTEX_POINT('',#35951);
#7496=VERTEX_POINT('',#35953);
#7497=VERTEX_POINT('',#35955);
#7498=VERTEX_POINT('',#35959);
#7499=VERTEX_POINT('',#35963);
#7500=VERTEX_POINT('',#35969);
#7501=VERTEX_POINT('',#35970);
#7502=VERTEX_POINT('',#35972);
#7503=VERTEX_POINT('',#35974);
#7504=VERTEX_POINT('',#35978);
#7505=VERTEX_POINT('',#35982);
#7506=VERTEX_POINT('',#35988);
#7507=VERTEX_POINT('',#35989);
#7508=VERTEX_POINT('',#35991);
#7509=VERTEX_POINT('',#35993);
#7510=VERTEX_POINT('',#35997);
#7511=VERTEX_POINT('',#36001);
#7512=VERTEX_POINT('',#36007);
#7513=VERTEX_POINT('',#36008);
#7514=VERTEX_POINT('',#36010);
#7515=VERTEX_POINT('',#36012);
#7516=VERTEX_POINT('',#36016);
#7517=VERTEX_POINT('',#36020);
#7518=VERTEX_POINT('',#36026);
#7519=VERTEX_POINT('',#36027);
#7520=VERTEX_POINT('',#36029);
#7521=VERTEX_POINT('',#36031);
#7522=VERTEX_POINT('',#36035);
#7523=VERTEX_POINT('',#36039);
#7524=VERTEX_POINT('',#36045);
#7525=VERTEX_POINT('',#36046);
#7526=VERTEX_POINT('',#36048);
#7527=VERTEX_POINT('',#36050);
#7528=VERTEX_POINT('',#36054);
#7529=VERTEX_POINT('',#36058);
#7530=VERTEX_POINT('',#36064);
#7531=VERTEX_POINT('',#36065);
#7532=VERTEX_POINT('',#36067);
#7533=VERTEX_POINT('',#36069);
#7534=VERTEX_POINT('',#36073);
#7535=VERTEX_POINT('',#36077);
#7536=VERTEX_POINT('',#36083);
#7537=VERTEX_POINT('',#36084);
#7538=VERTEX_POINT('',#36086);
#7539=VERTEX_POINT('',#36088);
#7540=VERTEX_POINT('',#36092);
#7541=VERTEX_POINT('',#36096);
#7542=VERTEX_POINT('',#36102);
#7543=VERTEX_POINT('',#36103);
#7544=VERTEX_POINT('',#36105);
#7545=VERTEX_POINT('',#36107);
#7546=VERTEX_POINT('',#36111);
#7547=VERTEX_POINT('',#36113);
#7548=VERTEX_POINT('',#36117);
#7549=VERTEX_POINT('',#36119);
#7550=VERTEX_POINT('',#36123);
#7551=VERTEX_POINT('',#36125);
#7552=VERTEX_POINT('',#36129);
#7553=VERTEX_POINT('',#36131);
#7554=VERTEX_POINT('',#36139);
#7555=VERTEX_POINT('',#36146);
#7556=VERTEX_POINT('',#36149);
#7557=VERTEX_POINT('',#36154);
#7558=VERTEX_POINT('',#36160);
#7559=VERTEX_POINT('',#36161);
#7560=VERTEX_POINT('',#36163);
#7561=VERTEX_POINT('',#36180);
#7562=VERTEX_POINT('',#36193);
#7563=VERTEX_POINT('',#36194);
#7564=VERTEX_POINT('',#36283);
#7565=VERTEX_POINT('',#36284);
#7566=VERTEX_POINT('',#36367);
#7567=VERTEX_POINT('',#36368);
#7568=VERTEX_POINT('',#36457);
#7569=VERTEX_POINT('',#36458);
#7570=VERTEX_POINT('',#36547);
#7571=VERTEX_POINT('',#36548);
#7572=VERTEX_POINT('',#36637);
#7573=VERTEX_POINT('',#36638);
#7574=VERTEX_POINT('',#36721);
#7575=VERTEX_POINT('',#36722);
#7576=VERTEX_POINT('',#36724);
#7577=VERTEX_POINT('',#36732);
#7578=VERTEX_POINT('',#36733);
#7579=VERTEX_POINT('',#36751);
#7580=VERTEX_POINT('',#36769);
#7581=VERTEX_POINT('',#36770);
#7582=VERTEX_POINT('',#36806);
#7583=VERTEX_POINT('',#36807);
#7584=VERTEX_POINT('',#36844);
#7585=VERTEX_POINT('',#36845);
#7586=VERTEX_POINT('',#36882);
#7587=VERTEX_POINT('',#36883);
#7588=VERTEX_POINT('',#36919);
#7589=VERTEX_POINT('',#36920);
#7590=VERTEX_POINT('',#36956);
#7591=VERTEX_POINT('',#36957);
#7592=VERTEX_POINT('',#36959);
#7593=VERTEX_POINT('',#36963);
#7594=VERTEX_POINT('',#36964);
#7595=VERTEX_POINT('',#36969);
#7596=VERTEX_POINT('',#36970);
#7597=VERTEX_POINT('',#36972);
#7598=VERTEX_POINT('',#36976);
#7599=VERTEX_POINT('',#36977);
#7600=VERTEX_POINT('',#36985);
#7601=VERTEX_POINT('',#36986);
#7602=VERTEX_POINT('',#36988);
#7603=VERTEX_POINT('',#36992);
#7604=VERTEX_POINT('',#36993);
#7605=VERTEX_POINT('',#36998);
#7606=VERTEX_POINT('',#36999);
#7607=VERTEX_POINT('',#37001);
#7608=VERTEX_POINT('',#37005);
#7609=VERTEX_POINT('',#37006);
#7610=VERTEX_POINT('',#37014);
#7611=VERTEX_POINT('',#37015);
#7612=VERTEX_POINT('',#37017);
#7613=VERTEX_POINT('',#37021);
#7614=VERTEX_POINT('',#37022);
#7615=VERTEX_POINT('',#37027);
#7616=VERTEX_POINT('',#37028);
#7617=VERTEX_POINT('',#37030);
#7618=VERTEX_POINT('',#37034);
#7619=VERTEX_POINT('',#37035);
#7620=VERTEX_POINT('',#37058);
#7621=VERTEX_POINT('',#37059);
#7622=VERTEX_POINT('',#37061);
#7623=VERTEX_POINT('',#37063);
#7624=VERTEX_POINT('',#37065);
#7625=VERTEX_POINT('',#37067);
#7626=VERTEX_POINT('',#37071);
#7627=VERTEX_POINT('',#37073);
#7628=VERTEX_POINT('',#37077);
#7629=VERTEX_POINT('',#37081);
#7630=VERTEX_POINT('',#37083);
#7631=VERTEX_POINT('',#37087);
#7632=VERTEX_POINT('',#37095);
#7633=VERTEX_POINT('',#37097);
#7634=VERTEX_POINT('',#37101);
#7635=VERTEX_POINT('',#37105);
#7636=VERTEX_POINT('',#37480);
#7637=VERTEX_POINT('',#37624);
#7638=VERTEX_POINT('',#37759);
#7639=VERTEX_POINT('',#37762);
#7640=VERTEX_POINT('',#38267);
#7641=VERTEX_POINT('',#38407);
#7642=VERTEX_POINT('',#38410);
#7643=VERTEX_POINT('',#38414);
#7644=VERTEX_POINT('',#38427);
#7645=VERTEX_POINT('',#38430);
#7646=VERTEX_POINT('',#38432);
#7647=VERTEX_POINT('',#38437);
#7648=EDGE_CURVE('',#6271,#6271,#5670,.T.);
#7649=EDGE_CURVE('',#6271,#6272,#3532,.T.);
#7650=EDGE_CURVE('',#6272,#6272,#5671,.T.);
#7651=EDGE_CURVE('',#6272,#6273,#3533,.T.);
#7652=EDGE_CURVE('',#6274,#6273,#5672,.T.);
#7653=EDGE_CURVE('',#6275,#6274,#1009,.T.);
#7654=EDGE_CURVE('',#6273,#6275,#5673,.T.);
#7655=EDGE_CURVE('',#6276,#6276,#5674,.T.);
#7656=EDGE_CURVE('',#6277,#6277,#5675,.T.);
#7657=EDGE_CURVE('',#6277,#6278,#3534,.T.);
#7658=EDGE_CURVE('',#6278,#6278,#5676,.T.);
#7659=EDGE_CURVE('',#6279,#6280,#3535,.T.);
#7660=EDGE_CURVE('',#6281,#6279,#5677,.T.);
#7661=EDGE_CURVE('',#6281,#6282,#3536,.T.);
#7662=EDGE_CURVE('',#6283,#6282,#5678,.T.);
#7663=EDGE_CURVE('',#6284,#6283,#3537,.T.);
#7664=EDGE_CURVE('',#6280,#6284,#5679,.T.);
#7665=EDGE_CURVE('',#6285,#6285,#5680,.T.);
#7666=EDGE_CURVE('',#6285,#6278,#3538,.T.);
#7667=EDGE_CURVE('',#6286,#6286,#5681,.T.);
#7668=EDGE_CURVE('',#6286,#6287,#3539,.T.);
#7669=EDGE_CURVE('',#6287,#6287,#5682,.T.);
#7670=EDGE_CURVE('',#6288,#6288,#5683,.T.);
#7671=EDGE_CURVE('',#6287,#6289,#3540,.T.);
#7672=EDGE_CURVE('',#6290,#6289,#5684,.T.);
#7673=EDGE_CURVE('',#6291,#6290,#1010,.T.);
#7674=EDGE_CURVE('',#6289,#6291,#5685,.T.);
#7675=EDGE_CURVE('',#6292,#6292,#5686,.T.);
#7676=EDGE_CURVE('',#6292,#6293,#3541,.T.);
#7677=EDGE_CURVE('',#6293,#6293,#5687,.T.);
#7678=EDGE_CURVE('',#6294,#6295,#3542,.T.);
#7679=EDGE_CURVE('',#6296,#6294,#5688,.T.);
#7680=EDGE_CURVE('',#6297,#6296,#3543,.T.);
#7681=EDGE_CURVE('',#6298,#6297,#5689,.T.);
#7682=EDGE_CURVE('',#6298,#6299,#3544,.T.);
#7683=EDGE_CURVE('',#6295,#6299,#5690,.T.);
#7684=EDGE_CURVE('',#6300,#6300,#5691,.T.);
#7685=EDGE_CURVE('',#6300,#6293,#3545,.T.);
#7686=EDGE_CURVE('',#6288,#6301,#3546,.T.);
#7687=EDGE_CURVE('',#6301,#6301,#5692,.T.);
#7688=EDGE_CURVE('',#6301,#6302,#3547,.T.);
#7689=EDGE_CURVE('',#6303,#6302,#1011,.T.);
#7690=EDGE_CURVE('',#6303,#6304,#5693,.T.);
#7691=EDGE_CURVE('',#6302,#6304,#1012,.T.);
#7692=EDGE_CURVE('',#6305,#6305,#5694,.T.);
#7693=EDGE_CURVE('',#6305,#6306,#3548,.T.);
#7694=EDGE_CURVE('',#6306,#6306,#5695,.T.);
#7695=EDGE_CURVE('',#6307,#6308,#3549,.T.);
#7696=EDGE_CURVE('',#6309,#6307,#5696,.T.);
#7697=EDGE_CURVE('',#6310,#6309,#3550,.T.);
#7698=EDGE_CURVE('',#6311,#6310,#5697,.T.);
#7699=EDGE_CURVE('',#6312,#6311,#3551,.T.);
#7700=EDGE_CURVE('',#6313,#6312,#5698,.T.);
#7701=EDGE_CURVE('',#6314,#6313,#3552,.T.);
#7702=EDGE_CURVE('',#6308,#6314,#5699,.T.);
#7703=EDGE_CURVE('',#6315,#6315,#5700,.T.);
#7704=EDGE_CURVE('',#6316,#6316,#5701,.T.);
#7705=EDGE_CURVE('',#6317,#6317,#5702,.T.);
#7706=EDGE_CURVE('',#6318,#6318,#5703,.T.);
#7707=EDGE_CURVE('',#6306,#6319,#3553,.T.);
#7708=EDGE_CURVE('',#6319,#6319,#5704,.T.);
#7709=EDGE_CURVE('',#6315,#6320,#3554,.T.);
#7710=EDGE_CURVE('',#6320,#6320,#5705,.T.);
#7711=EDGE_CURVE('',#6320,#6321,#3555,.T.);
#7712=EDGE_CURVE('',#6321,#6321,#5706,.T.);
#7713=EDGE_CURVE('',#6318,#6322,#3556,.T.);
#7714=EDGE_CURVE('',#6322,#6322,#5707,.T.);
#7715=EDGE_CURVE('',#6322,#6323,#3557,.T.);
#7716=EDGE_CURVE('',#6323,#6323,#5708,.T.);
#7717=EDGE_CURVE('',#6316,#6324,#3558,.T.);
#7718=EDGE_CURVE('',#6324,#6324,#5709,.T.);
#7719=EDGE_CURVE('',#6324,#6325,#3559,.T.);
#7720=EDGE_CURVE('',#6325,#6325,#5710,.T.);
#7721=EDGE_CURVE('',#6279,#6326,#1013,.F.);
#7722=EDGE_CURVE('',#6326,#6327,#5711,.T.);
#7723=EDGE_CURVE('',#6327,#6328,#1014,.T.);
#7724=EDGE_CURVE('',#6328,#6281,#332,.T.);
#7725=EDGE_CURVE('',#6327,#6329,#3560,.T.);
#7726=EDGE_CURVE('',#6329,#6330,#293,.F.);
#7727=EDGE_CURVE('',#6330,#6328,#3561,.T.);
#7728=EDGE_CURVE('',#6331,#6330,#3562,.T.);
#7729=EDGE_CURVE('',#6331,#6332,#3563,.T.);
#7730=EDGE_CURVE('',#6333,#6332,#3564,.T.);
#7731=EDGE_CURVE('',#6334,#6333,#3565,.T.);
#7732=EDGE_CURVE('',#6335,#6334,#3566,.T.);
#7733=EDGE_CURVE('',#6336,#6335,#3567,.T.);
#7734=EDGE_CURVE('',#6282,#6336,#333,.T.);
#7735=EDGE_CURVE('',#6337,#6338,#1015,.F.);
#7736=EDGE_CURVE('',#6338,#6339,#3568,.T.);
#7737=EDGE_CURVE('',#6339,#6340,#294,.F.);
#7738=EDGE_CURVE('',#6340,#6337,#3569,.T.);
#7739=EDGE_CURVE('',#6339,#6341,#3570,.T.);
#7740=EDGE_CURVE('',#6342,#6338,#1016,.F.);
#7741=EDGE_CURVE('',#6343,#6342,#3571,.T.);
#7742=EDGE_CURVE('',#6344,#6343,#1017,.F.);
#7743=EDGE_CURVE('',#6345,#6344,#3572,.T.);
#7744=EDGE_CURVE('',#6346,#6345,#3573,.T.);
#7745=EDGE_CURVE('',#6346,#6274,#3574,.T.);
#7746=EDGE_CURVE('',#6275,#6347,#3575,.T.);
#7747=EDGE_CURVE('',#6348,#6347,#3576,.T.);
#7748=EDGE_CURVE('',#6341,#6348,#3577,.T.);
#7749=EDGE_CURVE('',#6349,#6345,#295,.F.);
#7750=EDGE_CURVE('',#6344,#6350,#1018,.F.);
#7751=EDGE_CURVE('',#6350,#6349,#3578,.T.);
#7752=EDGE_CURVE('',#6351,#6352,#5712,.T.);
#7753=EDGE_CURVE('',#6352,#6295,#1019,.F.);
#7754=EDGE_CURVE('',#6299,#6353,#334,.T.);
#7755=EDGE_CURVE('',#6353,#6351,#1020,.T.);
#7756=EDGE_CURVE('',#6353,#6354,#3579,.T.);
#7757=EDGE_CURVE('',#6354,#6355,#296,.F.);
#7758=EDGE_CURVE('',#6355,#6351,#3580,.T.);
#7759=EDGE_CURVE('',#6356,#6326,#1021,.F.);
#7760=EDGE_CURVE('',#6357,#6356,#3581,.T.);
#7761=EDGE_CURVE('',#6358,#6357,#5713,.T.);
#7762=EDGE_CURVE('',#6358,#6359,#3582,.T.);
#7763=EDGE_CURVE('',#6352,#6359,#1022,.F.);
#7764=EDGE_CURVE('',#6355,#6360,#1023,.T.);
#7765=EDGE_CURVE('',#6361,#6360,#5714,.T.);
#7766=EDGE_CURVE('',#6349,#6361,#1024,.F.);
#7767=EDGE_CURVE('',#6337,#6350,#5715,.T.);
#7768=EDGE_CURVE('',#6340,#6362,#1025,.T.);
#7769=EDGE_CURVE('',#6363,#6362,#5716,.T.);
#7770=EDGE_CURVE('',#6329,#6363,#1026,.F.);
#7771=EDGE_CURVE('',#6297,#6364,#1027,.F.);
#7772=EDGE_CURVE('',#6364,#6365,#5717,.T.);
#7773=EDGE_CURVE('',#6365,#6366,#1028,.T.);
#7774=EDGE_CURVE('',#6366,#6298,#335,.T.);
#7775=EDGE_CURVE('',#6365,#6367,#3583,.T.);
#7776=EDGE_CURVE('',#6367,#6368,#297,.F.);
#7777=EDGE_CURVE('',#6368,#6366,#3584,.T.);
#7778=EDGE_CURVE('',#6369,#6368,#3585,.T.);
#7779=EDGE_CURVE('',#6369,#6370,#3586,.T.);
#7780=EDGE_CURVE('',#6371,#6370,#3587,.T.);
#7781=EDGE_CURVE('',#6372,#6371,#3588,.T.);
#7782=EDGE_CURVE('',#6354,#6372,#3589,.T.);
#7783=EDGE_CURVE('',#6373,#6374,#1029,.F.);
#7784=EDGE_CURVE('',#6374,#6375,#3590,.T.);
#7785=EDGE_CURVE('',#6375,#6376,#298,.F.);
#7786=EDGE_CURVE('',#6376,#6373,#3591,.T.);
#7787=EDGE_CURVE('',#6375,#6377,#3592,.T.);
#7788=EDGE_CURVE('',#6378,#6374,#1030,.F.);
#7789=EDGE_CURVE('',#6379,#6378,#3593,.T.);
#7790=EDGE_CURVE('',#6380,#6379,#1031,.F.);
#7791=EDGE_CURVE('',#6381,#6380,#3594,.T.);
#7792=EDGE_CURVE('',#6382,#6381,#3595,.T.);
#7793=EDGE_CURVE('',#6382,#6383,#3596,.T.);
#7794=EDGE_CURVE('',#6384,#6383,#3597,.T.);
#7795=EDGE_CURVE('',#6290,#6384,#3598,.T.);
#7796=EDGE_CURVE('',#6377,#6291,#3599,.T.);
#7797=EDGE_CURVE('',#6385,#6381,#299,.F.);
#7798=EDGE_CURVE('',#6380,#6386,#1032,.F.);
#7799=EDGE_CURVE('',#6386,#6385,#3600,.T.);
#7800=EDGE_CURVE('',#6387,#6388,#5718,.T.);
#7801=EDGE_CURVE('',#6388,#6283,#1033,.F.);
#7802=EDGE_CURVE('',#6336,#6387,#1034,.T.);
#7803=EDGE_CURVE('',#6335,#6389,#300,.F.);
#7804=EDGE_CURVE('',#6389,#6387,#3601,.T.);
#7805=EDGE_CURVE('',#6390,#6364,#1035,.F.);
#7806=EDGE_CURVE('',#6391,#6390,#3602,.T.);
#7807=EDGE_CURVE('',#6392,#6391,#5719,.T.);
#7808=EDGE_CURVE('',#6392,#6393,#3603,.T.);
#7809=EDGE_CURVE('',#6388,#6393,#1036,.F.);
#7810=EDGE_CURVE('',#6389,#6394,#1037,.T.);
#7811=EDGE_CURVE('',#6395,#6394,#5720,.T.);
#7812=EDGE_CURVE('',#6385,#6395,#1038,.F.);
#7813=EDGE_CURVE('',#6373,#6386,#5721,.T.);
#7814=EDGE_CURVE('',#6376,#6396,#1039,.T.);
#7815=EDGE_CURVE('',#6397,#6396,#5722,.T.);
#7816=EDGE_CURVE('',#6367,#6397,#1040,.F.);
#7817=EDGE_CURVE('',#6398,#6398,#5723,.T.);
#7818=EDGE_CURVE('',#6398,#6300,#3604,.T.);
#7819=EDGE_CURVE('',#6399,#6400,#5724,.T.);
#7820=EDGE_CURVE('',#6401,#6399,#3605,.T.);
#7821=EDGE_CURVE('',#6402,#6401,#5725,.T.);
#7822=EDGE_CURVE('',#6403,#6402,#3606,.T.);
#7823=EDGE_CURVE('',#6404,#6403,#5726,.T.);
#7824=EDGE_CURVE('',#6405,#6404,#3607,.T.);
#7825=EDGE_CURVE('',#6406,#6405,#5727,.T.);
#7826=EDGE_CURVE('',#6400,#6406,#3608,.T.);
#7827=EDGE_CURVE('',#6407,#6407,#5728,.T.);
#7828=EDGE_CURVE('',#6408,#6408,#5729,.T.);
#7829=EDGE_CURVE('',#6407,#6285,#3609,.T.);
#7830=EDGE_CURVE('',#6391,#6404,#1041,.F.);
#7831=EDGE_CURVE('',#6403,#6392,#1042,.T.);
#7832=EDGE_CURVE('',#6402,#6409,#5730,.T.);
#7833=EDGE_CURVE('',#6409,#6392,#3610,.T.);
#7834=EDGE_CURVE('',#6401,#6410,#5731,.T.);
#7835=EDGE_CURVE('',#6410,#6409,#5732,.T.);
#7836=EDGE_CURVE('',#6399,#6357,#1043,.F.);
#7837=EDGE_CURVE('',#6357,#6410,#3611,.T.);
#7838=EDGE_CURVE('',#6400,#6358,#1044,.T.);
#7839=EDGE_CURVE('',#6411,#6406,#5733,.T.);
#7840=EDGE_CURVE('',#6405,#6412,#5734,.T.);
#7841=EDGE_CURVE('',#6412,#6411,#5735,.T.);
#7842=EDGE_CURVE('',#6391,#6412,#3612,.T.);
#7843=EDGE_CURVE('',#6411,#6358,#3613,.T.);
#7844=EDGE_CURVE('',#6412,#6413,#3614,.T.);
#7845=EDGE_CURVE('',#6414,#6413,#5736,.T.);
#7846=EDGE_CURVE('',#6411,#6414,#3615,.T.);
#7847=EDGE_CURVE('',#6413,#6390,#3616,.T.);
#7848=EDGE_CURVE('',#6379,#6378,#5737,.T.);
#7849=EDGE_CURVE('',#6415,#6284,#5738,.T.);
#7850=EDGE_CURVE('',#6393,#6415,#3617,.T.);
#7851=EDGE_CURVE('',#6416,#6280,#5739,.T.);
#7852=EDGE_CURVE('',#6415,#6416,#5740,.T.);
#7853=EDGE_CURVE('',#6416,#6356,#3618,.T.);
#7854=EDGE_CURVE('',#6410,#6416,#3619,.T.);
#7855=EDGE_CURVE('',#6409,#6415,#3620,.T.);
#7856=EDGE_CURVE('',#6343,#6342,#5741,.T.);
#7857=EDGE_CURVE('',#6414,#6294,#5742,.T.);
#7858=EDGE_CURVE('',#6359,#6414,#3621,.T.);
#7859=EDGE_CURVE('',#6413,#6296,#5743,.T.);
#7860=EDGE_CURVE('',#6417,#6417,#5744,.T.);
#7861=EDGE_CURVE('',#6417,#6418,#5745,.T.);
#7862=EDGE_CURVE('',#6418,#6418,#5746,.T.);
#7863=EDGE_CURVE('',#6408,#6417,#3622,.T.);
#7864=EDGE_CURVE('',#6395,#6419,#3623,.T.);
#7865=EDGE_CURVE('',#6419,#6382,#5747,.T.);
#7866=EDGE_CURVE('',#6420,#6334,#5748,.T.);
#7867=EDGE_CURVE('',#6334,#6382,#5749,.T.);
#7868=EDGE_CURVE('',#6419,#6420,#5750,.T.);
#7869=EDGE_CURVE('',#6420,#6394,#3624,.T.);
#7870=EDGE_CURVE('',#6369,#6421,#5751,.T.);
#7871=EDGE_CURVE('',#6421,#6422,#5752,.T.);
#7872=EDGE_CURVE('',#6422,#6377,#5753,.T.);
#7873=EDGE_CURVE('',#6377,#6369,#5754,.T.);
#7874=EDGE_CURVE('',#6422,#6396,#3625,.T.);
#7875=EDGE_CURVE('',#6397,#6421,#3626,.T.);
#7876=EDGE_CURVE('',#6361,#6423,#3627,.T.);
#7877=EDGE_CURVE('',#6423,#6346,#5755,.T.);
#7878=EDGE_CURVE('',#6424,#6372,#5756,.T.);
#7879=EDGE_CURVE('',#6372,#6346,#5757,.T.);
#7880=EDGE_CURVE('',#6423,#6424,#5758,.T.);
#7881=EDGE_CURVE('',#6424,#6360,#3628,.T.);
#7882=EDGE_CURVE('',#6363,#6425,#3629,.T.);
#7883=EDGE_CURVE('',#6425,#6331,#5759,.T.);
#7884=EDGE_CURVE('',#6426,#6341,#5760,.T.);
#7885=EDGE_CURVE('',#6341,#6331,#5761,.T.);
#7886=EDGE_CURVE('',#6425,#6426,#5762,.T.);
#7887=EDGE_CURVE('',#6426,#6362,#3630,.T.);
#7888=EDGE_CURVE('',#6308,#6348,#5763,.T.);
#7889=EDGE_CURVE('',#6347,#6307,#5764,.T.);
#7890=EDGE_CURVE('',#6371,#6309,#5765,.T.);
#7891=EDGE_CURVE('',#6347,#6371,#5766,.T.);
#7892=EDGE_CURVE('',#6370,#6310,#5767,.T.);
#7893=EDGE_CURVE('',#6384,#6311,#5768,.T.);
#7894=EDGE_CURVE('',#6370,#6384,#5769,.T.);
#7895=EDGE_CURVE('',#6383,#6312,#5770,.T.);
#7896=EDGE_CURVE('',#6333,#6313,#5771,.T.);
#7897=EDGE_CURVE('',#6383,#6333,#5772,.T.);
#7898=EDGE_CURVE('',#6332,#6314,#5773,.T.);
#7899=EDGE_CURVE('',#6332,#6348,#5774,.T.);
#7900=EDGE_CURVE('',#6317,#6427,#5775,.T.);
#7901=EDGE_CURVE('',#6427,#6428,#5776,.T.);
#7902=EDGE_CURVE('',#6428,#6427,#5777,.T.);
#7903=EDGE_CURVE('',#6429,#6429,#5778,.T.);
#7904=EDGE_CURVE('',#6429,#6428,#3631,.T.);
#7905=EDGE_CURVE('',#6430,#6431,#1045,.T.);
#7906=EDGE_CURVE('',#6432,#6430,#1046,.T.);
#7907=EDGE_CURVE('',#6433,#6432,#1047,.T.);
#7908=EDGE_CURVE('',#6431,#6433,#1048,.T.);
#7909=EDGE_CURVE('',#6434,#6435,#1049,.T.);
#7910=EDGE_CURVE('',#6436,#6434,#1050,.T.);
#7911=EDGE_CURVE('',#6437,#6436,#1051,.T.);
#7912=EDGE_CURVE('',#6435,#6437,#1052,.T.);
#7913=EDGE_CURVE('',#6432,#6303,#5779,.T.);
#7914=EDGE_CURVE('',#6433,#6303,#1053,.F.);
#7915=EDGE_CURVE('',#6430,#6304,#5780,.T.);
#7916=EDGE_CURVE('',#6304,#6431,#1054,.F.);
#7917=EDGE_CURVE('',#6436,#6438,#5781,.T.);
#7918=EDGE_CURVE('',#6437,#6438,#1055,.F.);
#7919=EDGE_CURVE('',#6434,#6439,#5782,.T.);
#7920=EDGE_CURVE('',#6438,#6439,#5783,.T.);
#7921=EDGE_CURVE('',#6439,#6435,#1056,.F.);
#7922=EDGE_CURVE('',#6438,#6440,#1057,.T.);
#7923=EDGE_CURVE('',#6440,#6439,#1058,.T.);
#7924=EDGE_CURVE('',#6276,#6440,#3632,.T.);
#7925=EDGE_CURVE('',#6441,#6441,#5784,.T.);
#7926=EDGE_CURVE('',#6441,#6442,#3633,.T.);
#7927=EDGE_CURVE('',#6442,#6442,#5785,.T.);
#7928=EDGE_CURVE('',#6443,#6443,#5786,.T.);
#7929=EDGE_CURVE('',#6443,#6444,#3634,.T.);
#7930=EDGE_CURVE('',#6444,#6444,#5787,.T.);
#7931=EDGE_CURVE('',#6445,#6445,#5788,.T.);
#7932=EDGE_CURVE('',#6445,#6446,#3635,.T.);
#7933=EDGE_CURVE('',#6446,#6446,#5789,.T.);
#7934=EDGE_CURVE('',#6447,#6447,#5790,.T.);
#7935=EDGE_CURVE('',#6447,#6448,#3636,.T.);
#7936=EDGE_CURVE('',#6448,#6449,#5791,.T.);
#7937=EDGE_CURVE('',#6449,#6448,#5792,.T.);
#7938=EDGE_CURVE('',#6450,#6450,#5793,.T.);
#7939=EDGE_CURVE('',#6449,#6451,#3637,.T.);
#7940=EDGE_CURVE('',#6451,#6451,#5794,.T.);
#7941=EDGE_CURVE('',#6452,#6452,#5795,.T.);
#7942=EDGE_CURVE('',#6452,#6453,#3638,.T.);
#7943=EDGE_CURVE('',#6453,#6453,#5796,.T.);
#7944=EDGE_CURVE('',#6454,#6455,#5797,.T.);
#7945=EDGE_CURVE('',#6456,#6454,#3639,.T.);
#7946=EDGE_CURVE('',#6457,#6456,#5798,.T.);
#7947=EDGE_CURVE('',#6458,#6457,#3640,.T.);
#7948=EDGE_CURVE('',#6459,#6458,#5799,.T.);
#7949=EDGE_CURVE('',#6460,#6459,#3641,.T.);
#7950=EDGE_CURVE('',#6461,#6460,#5800,.T.);
#7951=EDGE_CURVE('',#6455,#6461,#3642,.T.);
#7952=EDGE_CURVE('',#6453,#6462,#3643,.T.);
#7953=EDGE_CURVE('',#6463,#6462,#1059,.T.);
#7954=EDGE_CURVE('',#6463,#6463,#5801,.T.);
#7955=EDGE_CURVE('',#6464,#6463,#1060,.T.);
#7956=EDGE_CURVE('',#6462,#6464,#1061,.T.);
#7957=EDGE_CURVE('',#6455,#6465,#3644,.T.);
#7958=EDGE_CURVE('',#6465,#6466,#5802,.T.);
#7959=EDGE_CURVE('',#6466,#6467,#5803,.T.);
#7960=EDGE_CURVE('',#6467,#6454,#3645,.T.);
#7961=EDGE_CURVE('',#6468,#6469,#3646,.T.);
#7962=EDGE_CURVE('',#6469,#6470,#1062,.T.);
#7963=EDGE_CURVE('',#6470,#6471,#3647,.T.);
#7964=EDGE_CURVE('',#6471,#6468,#1063,.T.);
#7965=EDGE_CURVE('',#6470,#6454,#1064,.T.);
#7966=EDGE_CURVE('',#6467,#6471,#1065,.T.);
#7967=EDGE_CURVE('',#6472,#6473,#3648,.T.);
#7968=EDGE_CURVE('',#6473,#6474,#5804,.T.);
#7969=EDGE_CURVE('',#6474,#6475,#3649,.T.);
#7970=EDGE_CURVE('',#6475,#6472,#5805,.T.);
#7971=EDGE_CURVE('',#6472,#6469,#1066,.T.);
#7972=EDGE_CURVE('',#6468,#6473,#1067,.T.);
#7973=EDGE_CURVE('',#6476,#6477,#3650,.T.);
#7974=EDGE_CURVE('',#6477,#6478,#1068,.T.);
#7975=EDGE_CURVE('',#6478,#6479,#3651,.T.);
#7976=EDGE_CURVE('',#6479,#6476,#1069,.T.);
#7977=EDGE_CURVE('',#6478,#6475,#1070,.T.);
#7978=EDGE_CURVE('',#6474,#6479,#1071,.T.);
#7979=EDGE_CURVE('',#6455,#6477,#1072,.T.);
#7980=EDGE_CURVE('',#6476,#6465,#1073,.T.);
#7981=EDGE_CURVE('',#6480,#6475,#3652,.T.);
#7982=EDGE_CURVE('',#6472,#6480,#3653,.T.);
#7983=EDGE_CURVE('',#6481,#6461,#1074,.T.);
#7984=EDGE_CURVE('',#6482,#6481,#1075,.T.);
#7985=EDGE_CURVE('',#6483,#6482,#1076,.T.);
#7986=EDGE_CURVE('',#6483,#6484,#3654,.T.);
#7987=EDGE_CURVE('',#6485,#6484,#5806,.T.);
#7988=EDGE_CURVE('',#6485,#6486,#3655,.T.);
#7989=EDGE_CURVE('',#6480,#6486,#5807,.T.);
#7990=EDGE_CURVE('',#6466,#6487,#3656,.T.);
#7991=EDGE_CURVE('',#6487,#6487,#5808,.T.);
#7992=EDGE_CURVE('',#6456,#6488,#3657,.T.);
#7993=EDGE_CURVE('',#6488,#6489,#5809,.T.);
#7994=EDGE_CURVE('',#6489,#6457,#3658,.T.);
#7995=EDGE_CURVE('',#6490,#6491,#3659,.T.);
#7996=EDGE_CURVE('',#6491,#6492,#1077,.T.);
#7997=EDGE_CURVE('',#6492,#6493,#3660,.T.);
#7998=EDGE_CURVE('',#6493,#6494,#1078,.T.);
#7999=EDGE_CURVE('',#6494,#6490,#1079,.T.);
#8000=EDGE_CURVE('',#6492,#6457,#1080,.T.);
#8001=EDGE_CURVE('',#6489,#6493,#1081,.T.);
#8002=EDGE_CURVE('',#6495,#6496,#3661,.T.);
#8003=EDGE_CURVE('',#6496,#6497,#5810,.T.);
#8004=EDGE_CURVE('',#6497,#6498,#3662,.T.);
#8005=EDGE_CURVE('',#6498,#6495,#5811,.T.);
#8006=EDGE_CURVE('',#6495,#6491,#1082,.T.);
#8007=EDGE_CURVE('',#6490,#6496,#1083,.T.);
#8008=EDGE_CURVE('',#6499,#6500,#3663,.T.);
#8009=EDGE_CURVE('',#6500,#6501,#1084,.T.);
#8010=EDGE_CURVE('',#6501,#6502,#3664,.T.);
#8011=EDGE_CURVE('',#6502,#6499,#1085,.T.);
#8012=EDGE_CURVE('',#6501,#6498,#1086,.T.);
#8013=EDGE_CURVE('',#6497,#6502,#1087,.T.);
#8014=EDGE_CURVE('',#6456,#6500,#1088,.T.);
#8015=EDGE_CURVE('',#6499,#6488,#1089,.T.);
#8016=EDGE_CURVE('',#6503,#6498,#3665,.T.);
#8017=EDGE_CURVE('',#6495,#6503,#3666,.T.);
#8018=EDGE_CURVE('',#6480,#6504,#5812,.T.);
#8019=EDGE_CURVE('',#6504,#6505,#3667,.T.);
#8020=EDGE_CURVE('',#6505,#6503,#5813,.F.);
#8021=EDGE_CURVE('',#6494,#6506,#3668,.T.);
#8022=EDGE_CURVE('',#6506,#6506,#5814,.T.);
#8023=EDGE_CURVE('',#6483,#6507,#3669,.T.);
#8024=EDGE_CURVE('',#6507,#6508,#5815,.T.);
#8025=EDGE_CURVE('',#6508,#6509,#3670,.T.);
#8026=EDGE_CURVE('',#6509,#6483,#5816,.T.);
#8027=EDGE_CURVE('',#6510,#6511,#3671,.T.);
#8028=EDGE_CURVE('',#6511,#6512,#1090,.T.);
#8029=EDGE_CURVE('',#6512,#6513,#3672,.T.);
#8030=EDGE_CURVE('',#6513,#6510,#1091,.T.);
#8031=EDGE_CURVE('',#6512,#6509,#1092,.T.);
#8032=EDGE_CURVE('',#6508,#6513,#1093,.T.);
#8033=EDGE_CURVE('',#6460,#6514,#3673,.T.);
#8034=EDGE_CURVE('',#6514,#6515,#5817,.T.);
#8035=EDGE_CURVE('',#6515,#6516,#5818,.T.);
#8036=EDGE_CURVE('',#6516,#6461,#3674,.T.);
#8037=EDGE_CURVE('',#6460,#6511,#1094,.T.);
#8038=EDGE_CURVE('',#6510,#6514,#1095,.T.);
#8039=EDGE_CURVE('',#6517,#6482,#3675,.T.);
#8040=EDGE_CURVE('',#6481,#6518,#3676,.T.);
#8041=EDGE_CURVE('',#6518,#6517,#1096,.T.);
#8042=EDGE_CURVE('',#6516,#6518,#1097,.T.);
#8043=EDGE_CURVE('',#6517,#6507,#1098,.T.);
#8044=EDGE_CURVE('',#6515,#6519,#3677,.T.);
#8045=EDGE_CURVE('',#6519,#6519,#5819,.T.);
#8046=EDGE_CURVE('',#6458,#6520,#3678,.T.);
#8047=EDGE_CURVE('',#6520,#6521,#5820,.T.);
#8048=EDGE_CURVE('',#6521,#6459,#3679,.T.);
#8049=EDGE_CURVE('',#6522,#6523,#3680,.T.);
#8050=EDGE_CURVE('',#6523,#6524,#1099,.T.);
#8051=EDGE_CURVE('',#6524,#6525,#3681,.T.);
#8052=EDGE_CURVE('',#6525,#6522,#1100,.T.);
#8053=EDGE_CURVE('',#6524,#6459,#1101,.T.);
#8054=EDGE_CURVE('',#6521,#6525,#1102,.T.);
#8055=EDGE_CURVE('',#6526,#6527,#3682,.T.);
#8056=EDGE_CURVE('',#6527,#6528,#5821,.T.);
#8057=EDGE_CURVE('',#6528,#6529,#3683,.T.);
#8058=EDGE_CURVE('',#6529,#6526,#5822,.T.);
#8059=EDGE_CURVE('',#6526,#6523,#1103,.T.);
#8060=EDGE_CURVE('',#6522,#6527,#1104,.T.);
#8061=EDGE_CURVE('',#6530,#6531,#3684,.T.);
#8062=EDGE_CURVE('',#6531,#6532,#1105,.T.);
#8063=EDGE_CURVE('',#6532,#6533,#3685,.T.);
#8064=EDGE_CURVE('',#6533,#6534,#1106,.T.);
#8065=EDGE_CURVE('',#6534,#6530,#1107,.T.);
#8066=EDGE_CURVE('',#6532,#6529,#1108,.T.);
#8067=EDGE_CURVE('',#6528,#6533,#1109,.T.);
#8068=EDGE_CURVE('',#6458,#6531,#1110,.T.);
#8069=EDGE_CURVE('',#6530,#6520,#1111,.T.);
#8070=EDGE_CURVE('',#6535,#6529,#3686,.T.);
#8071=EDGE_CURVE('',#6526,#6535,#3687,.T.);
#8072=EDGE_CURVE('',#6503,#6536,#5823,.F.);
#8073=EDGE_CURVE('',#6536,#6537,#3688,.T.);
#8074=EDGE_CURVE('',#6537,#6535,#5824,.F.);
#8075=EDGE_CURVE('',#6534,#6538,#3689,.T.);
#8076=EDGE_CURVE('',#6538,#6538,#5825,.T.);
#8077=EDGE_CURVE('',#6539,#6540,#1112,.T.);
#8078=EDGE_CURVE('',#6539,#6541,#1113,.T.);
#8079=EDGE_CURVE('',#6541,#6542,#1114,.T.);
#8080=EDGE_CURVE('',#6542,#6540,#1115,.T.);
#8081=EDGE_CURVE('',#6541,#6543,#1116,.T.);
#8082=EDGE_CURVE('',#6543,#6544,#3690,.T.);
#8083=EDGE_CURVE('',#6544,#6542,#1117,.T.);
#8084=EDGE_CURVE('',#6540,#6545,#1118,.T.);
#8085=EDGE_CURVE('',#6545,#6546,#1119,.T.);
#8086=EDGE_CURVE('',#6546,#6547,#1120,.T.);
#8087=EDGE_CURVE('',#6547,#6539,#1121,.T.);
#8088=EDGE_CURVE('',#6548,#6549,#1122,.F.);
#8089=EDGE_CURVE('',#6549,#6550,#5826,.T.);
#8090=EDGE_CURVE('',#6550,#6551,#3691,.T.);
#8091=EDGE_CURVE('',#6551,#6548,#5827,.T.);
#8092=EDGE_CURVE('',#6550,#6544,#1123,.T.);
#8093=EDGE_CURVE('',#6543,#6551,#1124,.T.);
#8094=EDGE_CURVE('',#6545,#6552,#1125,.T.);
#8095=EDGE_CURVE('',#6552,#6547,#1126,.T.);
#8096=EDGE_CURVE('',#6553,#6549,#1127,.F.);
#8097=EDGE_CURVE('',#6553,#6554,#3692,.T.);
#8098=EDGE_CURVE('',#6554,#6555,#1128,.T.);
#8099=EDGE_CURVE('',#6555,#6556,#5828,.F.);
#8100=EDGE_CURVE('',#6556,#6552,#3693,.T.);
#8101=EDGE_CURVE('',#6557,#6558,#1129,.T.);
#8102=EDGE_CURVE('',#6557,#6559,#1130,.T.);
#8103=EDGE_CURVE('',#6559,#6560,#1131,.T.);
#8104=EDGE_CURVE('',#6560,#6561,#1132,.T.);
#8105=EDGE_CURVE('',#6561,#6558,#1133,.T.);
#8106=EDGE_CURVE('',#6558,#6562,#336,.T.);
#8107=EDGE_CURVE('',#6563,#6562,#1134,.T.);
#8108=EDGE_CURVE('',#6563,#6557,#337,.T.);
#8109=EDGE_CURVE('',#6562,#6564,#1135,.T.);
#8110=EDGE_CURVE('',#6564,#6565,#3694,.T.);
#8111=EDGE_CURVE('',#6565,#6563,#1136,.T.);
#8112=EDGE_CURVE('',#6566,#6567,#3695,.T.);
#8113=EDGE_CURVE('',#6567,#6568,#5829,.T.);
#8114=EDGE_CURVE('',#6568,#6569,#1137,.F.);
#8115=EDGE_CURVE('',#6569,#6566,#5830,.T.);
#8116=EDGE_CURVE('',#6566,#6565,#1138,.T.);
#8117=EDGE_CURVE('',#6564,#6567,#1139,.T.);
#8118=EDGE_CURVE('',#6559,#6570,#1140,.T.);
#8119=EDGE_CURVE('',#6570,#6561,#1141,.T.);
#8120=EDGE_CURVE('',#6566,#6571,#5831,.T.);
#8121=EDGE_CURVE('',#6571,#6572,#5832,.F.);
#8122=EDGE_CURVE('',#6572,#6570,#5833,.T.);
#8123=EDGE_CURVE('',#6573,#6551,#5834,.T.);
#8124=EDGE_CURVE('',#6574,#6573,#5835,.T.);
#8125=EDGE_CURVE('',#6575,#6574,#3696,.T.);
#8126=EDGE_CURVE('',#6576,#6575,#5836,.T.);
#8127=EDGE_CURVE('',#6577,#6576,#5837,.T.);
#8128=EDGE_CURVE('',#6578,#6577,#5838,.T.);
#8129=EDGE_CURVE('',#6579,#6578,#3697,.T.);
#8130=EDGE_CURVE('',#6580,#6579,#3698,.T.);
#8131=EDGE_CURVE('',#6581,#6580,#3699,.T.);
#8132=EDGE_CURVE('',#6582,#6581,#5839,.T.);
#8133=EDGE_CURVE('',#6583,#6582,#5840,.T.);
#8134=EDGE_CURVE('',#6584,#6583,#5841,.T.);
#8135=EDGE_CURVE('',#6585,#6584,#3700,.T.);
#8136=EDGE_CURVE('',#6571,#6585,#5842,.T.);
#8137=EDGE_CURVE('',#6486,#6569,#3701,.T.);
#8138=EDGE_CURVE('',#6485,#6548,#3702,.T.);
#8139=EDGE_CURVE('',#6586,#6586,#5843,.T.);
#8140=EDGE_CURVE('',#6586,#6587,#3703,.T.);
#8141=EDGE_CURVE('',#6587,#6587,#5844,.T.);
#8142=EDGE_CURVE('',#6588,#6589,#3704,.T.);
#8143=EDGE_CURVE('',#6590,#6588,#3705,.T.);
#8144=EDGE_CURVE('',#6591,#6590,#3706,.T.);
#8145=EDGE_CURVE('',#6589,#6591,#3707,.T.);
#8146=EDGE_CURVE('',#6592,#6592,#5845,.T.);
#8147=EDGE_CURVE('',#6593,#6593,#5846,.T.);
#8148=EDGE_CURVE('',#6594,#6594,#5847,.T.);
#8149=EDGE_CURVE('',#6595,#6595,#5848,.T.);
#8150=EDGE_CURVE('',#6587,#6596,#3708,.T.);
#8151=EDGE_CURVE('',#6596,#6596,#5849,.T.);
#8152=EDGE_CURVE('',#6592,#6597,#3709,.T.);
#8153=EDGE_CURVE('',#6597,#6597,#5850,.T.);
#8154=EDGE_CURVE('',#6597,#6598,#3710,.T.);
#8155=EDGE_CURVE('',#6598,#6598,#5851,.T.);
#8156=EDGE_CURVE('',#6595,#6599,#3711,.T.);
#8157=EDGE_CURVE('',#6599,#6599,#5852,.T.);
#8158=EDGE_CURVE('',#6599,#6600,#3712,.T.);
#8159=EDGE_CURVE('',#6600,#6600,#5853,.T.);
#8160=EDGE_CURVE('',#6593,#6601,#3713,.T.);
#8161=EDGE_CURVE('',#6601,#6601,#5854,.T.);
#8162=EDGE_CURVE('',#6601,#6602,#3714,.T.);
#8163=EDGE_CURVE('',#6602,#6602,#5855,.T.);
#8164=EDGE_CURVE('',#6594,#6603,#3715,.T.);
#8165=EDGE_CURVE('',#6603,#6603,#5856,.T.);
#8166=EDGE_CURVE('',#6603,#6604,#3716,.T.);
#8167=EDGE_CURVE('',#6605,#6604,#1142,.T.);
#8168=EDGE_CURVE('',#6605,#6605,#5857,.T.);
#8169=EDGE_CURVE('',#6606,#6605,#1143,.T.);
#8170=EDGE_CURVE('',#6604,#6606,#1144,.T.);
#8171=EDGE_CURVE('',#6606,#6607,#5858,.T.);
#8172=EDGE_CURVE('',#6607,#6607,#1145,.T.);
#8173=EDGE_CURVE('',#6608,#6608,#5859,.T.);
#8174=EDGE_CURVE('',#6608,#6607,#3717,.T.);
#8175=EDGE_CURVE('',#6609,#6610,#5860,.T.);
#8176=EDGE_CURVE('',#6610,#6611,#3718,.T.);
#8177=EDGE_CURVE('',#6611,#6612,#1146,.F.);
#8178=EDGE_CURVE('',#6612,#6609,#3719,.T.);
#8179=EDGE_CURVE('',#6588,#6613,#5861,.F.);
#8180=EDGE_CURVE('',#6614,#6588,#5862,.F.);
#8181=EDGE_CURVE('',#6613,#6614,#5863,.F.);
#8182=EDGE_CURVE('',#6589,#6609,#5864,.T.);
#8183=EDGE_CURVE('',#6609,#6614,#3720,.T.);
#8184=EDGE_CURVE('',#6615,#6616,#1147,.F.);
#8185=EDGE_CURVE('',#6616,#6613,#3721,.T.);
#8186=EDGE_CURVE('',#6614,#6615,#3722,.T.);
#8187=EDGE_CURVE('',#6617,#6590,#5865,.T.);
#8188=EDGE_CURVE('',#6613,#6617,#3723,.T.);
#8189=EDGE_CURVE('',#6589,#6610,#5866,.T.);
#8190=EDGE_CURVE('',#6580,#6617,#5867,.T.);
#8191=EDGE_CURVE('',#6617,#6618,#3724,.T.);
#8192=EDGE_CURVE('',#6618,#6581,#1148,.F.);
#8193=EDGE_CURVE('',#6580,#6590,#5868,.T.);
#8194=EDGE_CURVE('',#6619,#6610,#3725,.T.);
#8195=EDGE_CURVE('',#6620,#6619,#3726,.T.);
#8196=EDGE_CURVE('',#6611,#6620,#3727,.T.);
#8197=EDGE_CURVE('',#6591,#6619,#5869,.T.);
#8198=EDGE_CURVE('',#6591,#6579,#5870,.T.);
#8199=EDGE_CURVE('',#6536,#6505,#5871,.F.);
#8200=EDGE_CURVE('',#6621,#6537,#5872,.F.);
#8201=EDGE_CURVE('',#6535,#6621,#5873,.F.);
#8202=EDGE_CURVE('',#6622,#6623,#1149,.F.);
#8203=EDGE_CURVE('',#6623,#6621,#3728,.T.);
#8204=EDGE_CURVE('',#6537,#6622,#3729,.T.);
#8205=EDGE_CURVE('',#6621,#6624,#3730,.T.);
#8206=EDGE_CURVE('',#6624,#6484,#5874,.T.);
#8207=EDGE_CURVE('',#6484,#6509,#3731,.T.);
#8208=EDGE_CURVE('',#6624,#6485,#5875,.T.);
#8209=EDGE_CURVE('',#6486,#6504,#5876,.T.);
#8210=EDGE_CURVE('',#6625,#6626,#1150,.F.);
#8211=EDGE_CURVE('',#6626,#6536,#3732,.T.);
#8212=EDGE_CURVE('',#6505,#6625,#3733,.T.);
#8213=EDGE_CURVE('',#6624,#6553,#3734,.T.);
#8214=EDGE_CURVE('',#6554,#6623,#3735,.T.);
#8215=EDGE_CURVE('',#6627,#6612,#5877,.T.);
#8216=EDGE_CURVE('',#6628,#6627,#3736,.T.);
#8217=EDGE_CURVE('',#6622,#6628,#5878,.T.);
#8218=EDGE_CURVE('',#6629,#6626,#5879,.T.);
#8219=EDGE_CURVE('',#6630,#6629,#3737,.T.);
#8220=EDGE_CURVE('',#6615,#6630,#5880,.T.);
#8221=EDGE_CURVE('',#6631,#6631,#5881,.T.);
#8222=EDGE_CURVE('',#6632,#6632,#5882,.T.);
#8223=EDGE_CURVE('',#6633,#6633,#5883,.T.);
#8224=EDGE_CURVE('',#6634,#6634,#5884,.T.);
#8225=EDGE_CURVE('',#6635,#6635,#5885,.T.);
#8226=EDGE_CURVE('',#6631,#6636,#5886,.T.);
#8227=EDGE_CURVE('',#6636,#6637,#5887,.T.);
#8228=EDGE_CURVE('',#6637,#6636,#5888,.T.);
#8229=EDGE_CURVE('',#6637,#6638,#3738,.T.);
#8230=EDGE_CURVE('',#6638,#6638,#5889,.T.);
#8231=EDGE_CURVE('',#6628,#6639,#5890,.T.);
#8232=EDGE_CURVE('',#6639,#6623,#5891,.T.);
#8233=EDGE_CURVE('',#6627,#6640,#5892,.T.);
#8234=EDGE_CURVE('',#6640,#6639,#3739,.T.);
#8235=EDGE_CURVE('',#6611,#6640,#5893,.T.);
#8236=EDGE_CURVE('',#6464,#6641,#5894,.T.);
#8237=EDGE_CURVE('',#6641,#6642,#1151,.T.);
#8238=EDGE_CURVE('',#6642,#6463,#5895,.T.);
#8239=EDGE_CURVE('',#6642,#6641,#1152,.T.);
#8240=EDGE_CURVE('',#6643,#6643,#5896,.T.);
#8241=EDGE_CURVE('',#6554,#6644,#5897,.T.);
#8242=EDGE_CURVE('',#6644,#6645,#1153,.F.);
#8243=EDGE_CURVE('',#6645,#6555,#5898,.T.);
#8244=EDGE_CURVE('',#6646,#6645,#5899,.F.);
#8245=EDGE_CURVE('',#6556,#6646,#5900,.T.);
#8246=EDGE_CURVE('',#6647,#6647,#5901,.T.);
#8247=EDGE_CURVE('',#6648,#6649,#1154,.F.);
#8248=EDGE_CURVE('',#6649,#6650,#5902,.T.);
#8249=EDGE_CURVE('',#6650,#6651,#1155,.F.);
#8250=EDGE_CURVE('',#6651,#6648,#5903,.T.);
#8251=EDGE_CURVE('',#6652,#6651,#3740,.T.);
#8252=EDGE_CURVE('',#6653,#6652,#5904,.T.);
#8253=EDGE_CURVE('',#6654,#6653,#3741,.T.);
#8254=EDGE_CURVE('',#6625,#6654,#5905,.T.);
#8255=EDGE_CURVE('',#6625,#6648,#3742,.T.);
#8256=EDGE_CURVE('',#6655,#6656,#1156,.F.);
#8257=EDGE_CURVE('',#6656,#6657,#5906,.T.);
#8258=EDGE_CURVE('',#6657,#6658,#1157,.F.);
#8259=EDGE_CURVE('',#6658,#6655,#5907,.T.);
#8260=EDGE_CURVE('',#6659,#6656,#5908,.F.);
#8261=EDGE_CURVE('',#6660,#6659,#5909,.T.);
#8262=EDGE_CURVE('',#6657,#6660,#5910,.F.);
#8263=EDGE_CURVE('',#6661,#6661,#5911,.T.);
#8264=EDGE_CURVE('',#6662,#6663,#1158,.F.);
#8265=EDGE_CURVE('',#6663,#6664,#5912,.T.);
#8266=EDGE_CURVE('',#6664,#6665,#1159,.F.);
#8267=EDGE_CURVE('',#6665,#6662,#5913,.T.);
#8268=EDGE_CURVE('',#6666,#6663,#5914,.F.);
#8269=EDGE_CURVE('',#6667,#6666,#5915,.T.);
#8270=EDGE_CURVE('',#6664,#6667,#5916,.F.);
#8271=EDGE_CURVE('',#6668,#6668,#5917,.T.);
#8272=EDGE_CURVE('',#6669,#6630,#5918,.T.);
#8273=EDGE_CURVE('',#6629,#6654,#5919,.T.);
#8274=EDGE_CURVE('',#6654,#6669,#3743,.T.);
#8275=EDGE_CURVE('',#6669,#6616,#5920,.T.);
#8276=EDGE_CURVE('',#6670,#6665,#3744,.T.);
#8277=EDGE_CURVE('',#6618,#6670,#5921,.T.);
#8278=EDGE_CURVE('',#6618,#6616,#3745,.T.);
#8279=EDGE_CURVE('',#6669,#6671,#3746,.T.);
#8280=EDGE_CURVE('',#6672,#6671,#5922,.T.);
#8281=EDGE_CURVE('',#6662,#6672,#3747,.T.);
#8282=EDGE_CURVE('',#6671,#6653,#3748,.T.);
#8283=EDGE_CURVE('',#6673,#6574,#5923,.T.);
#8284=EDGE_CURVE('',#6573,#6674,#5924,.T.);
#8285=EDGE_CURVE('',#6674,#6673,#5925,.T.);
#8286=EDGE_CURVE('',#6675,#6575,#5926,.T.);
#8287=EDGE_CURVE('',#6673,#6675,#3749,.T.);
#8288=EDGE_CURVE('',#6676,#6576,#5927,.T.);
#8289=EDGE_CURVE('',#6675,#6676,#5928,.T.);
#8290=EDGE_CURVE('',#6676,#6677,#5929,.T.);
#8291=EDGE_CURVE('',#6677,#6576,#5930,.T.);
#8292=EDGE_CURVE('',#6573,#6678,#5931,.T.);
#8293=EDGE_CURVE('',#6678,#6674,#5932,.T.);
#8294=EDGE_CURVE('',#6677,#6679,#5933,.T.);
#8295=EDGE_CURVE('',#6679,#6577,#5934,.F.);
#8296=EDGE_CURVE('',#6676,#6658,#3750,.T.);
#8297=EDGE_CURVE('',#6660,#6677,#3751,.T.);
#8298=EDGE_CURVE('',#6680,#6620,#5935,.T.);
#8299=EDGE_CURVE('',#6655,#6680,#3752,.T.);
#8300=EDGE_CURVE('',#6640,#6675,#3753,.T.);
#8301=EDGE_CURVE('',#6639,#6673,#3754,.T.);
#8302=EDGE_CURVE('',#6644,#6674,#3755,.T.);
#8303=EDGE_CURVE('',#6568,#6681,#1160,.F.);
#8304=EDGE_CURVE('',#6681,#6504,#3756,.T.);
#8305=EDGE_CURVE('',#6648,#6681,#3757,.T.);
#8306=EDGE_CURVE('',#6619,#6579,#5936,.T.);
#8307=EDGE_CURVE('',#6578,#6620,#1161,.F.);
#8308=EDGE_CURVE('',#6552,#6678,#5937,.T.);
#8309=EDGE_CURVE('',#6678,#6646,#3758,.T.);
#8310=EDGE_CURVE('',#6570,#6682,#3759,.T.);
#8311=EDGE_CURVE('',#6649,#6682,#5938,.T.);
#8312=EDGE_CURVE('',#6683,#6572,#3760,.T.);
#8313=EDGE_CURVE('',#6683,#6682,#5939,.T.);
#8314=EDGE_CURVE('',#6684,#6670,#5940,.F.);
#8315=EDGE_CURVE('',#6582,#6684,#5941,.F.);
#8316=EDGE_CURVE('',#6670,#6582,#5942,.F.);
#8317=EDGE_CURVE('',#6672,#6685,#5943,.F.);
#8318=EDGE_CURVE('',#6583,#6672,#5944,.F.);
#8319=EDGE_CURVE('',#6685,#6583,#5945,.F.);
#8320=EDGE_CURVE('',#6572,#6652,#5946,.F.);
#8321=EDGE_CURVE('',#6652,#6571,#5947,.F.);
#8322=EDGE_CURVE('',#6671,#6584,#5948,.T.);
#8323=EDGE_CURVE('',#6653,#6585,#5949,.T.);
#8324=EDGE_CURVE('',#6650,#6683,#5950,.F.);
#8325=EDGE_CURVE('',#6684,#6685,#5951,.T.);
#8326=EDGE_CURVE('',#6685,#6666,#3761,.T.);
#8327=EDGE_CURVE('',#6667,#6684,#3762,.T.);
#8328=EDGE_CURVE('',#6680,#6679,#5952,.F.);
#8329=EDGE_CURVE('',#6577,#6680,#5953,.F.);
#8330=EDGE_CURVE('',#6679,#6659,#3763,.T.);
#8331=EDGE_CURVE('',#6661,#6635,#3764,.T.);
#8332=EDGE_CURVE('',#6686,#6686,#5954,.T.);
#8333=EDGE_CURVE('',#6686,#6634,#3765,.T.);
#8334=EDGE_CURVE('',#6668,#6633,#3766,.T.);
#8335=EDGE_CURVE('',#6647,#6632,#3767,.T.);
#8336=EDGE_CURVE('',#6643,#6687,#3768,.T.);
#8337=EDGE_CURVE('',#6687,#6687,#5955,.T.);
#8338=EDGE_CURVE('',#6688,#6688,#5956,.T.);
#8339=EDGE_CURVE('',#6688,#6450,#3769,.T.);
#8340=EDGE_CURVE('',#6689,#6690,#301,.T.);
#8341=EDGE_CURVE('',#6690,#6691,#3770,.T.);
#8342=EDGE_CURVE('',#6691,#6692,#302,.T.);
#8343=EDGE_CURVE('',#6692,#6689,#3771,.T.);
#8344=EDGE_CURVE('',#6690,#6693,#3772,.T.);
#8345=EDGE_CURVE('',#6694,#6693,#3773,.T.);
#8346=EDGE_CURVE('',#6694,#6691,#3774,.T.);
#8347=EDGE_CURVE('',#6695,#6689,#5957,.T.);
#8348=EDGE_CURVE('',#6696,#6695,#303,.T.);
#8349=EDGE_CURVE('',#6697,#6696,#3775,.T.);
#8350=EDGE_CURVE('',#6698,#6697,#304,.T.);
#8351=EDGE_CURVE('',#6699,#6698,#305,.T.);
#8352=EDGE_CURVE('',#6693,#6699,#306,.T.);
#8353=EDGE_CURVE('',#6700,#6694,#307,.T.);
#8354=EDGE_CURVE('',#6699,#6700,#3776,.T.);
#8355=EDGE_CURVE('',#6701,#6698,#3777,.T.);
#8356=EDGE_CURVE('',#6701,#6700,#308,.T.);
#8357=EDGE_CURVE('',#6702,#6702,#309,.T.);
#8358=EDGE_CURVE('',#6703,#6704,#310,.T.);
#8359=EDGE_CURVE('',#6704,#6696,#3778,.T.);
#8360=EDGE_CURVE('',#6695,#6703,#3779,.T.);
#8361=EDGE_CURVE('',#6692,#6703,#5958,.T.);
#8362=EDGE_CURVE('',#6705,#6705,#5959,.T.);
#8363=EDGE_CURVE('',#6697,#6706,#3780,.T.);
#8364=EDGE_CURVE('',#6706,#6701,#311,.T.);
#8365=EDGE_CURVE('',#6704,#6706,#3781,.T.);
#8366=EDGE_CURVE('',#6705,#6702,#3782,.T.);
#8367=EDGE_CURVE('',#6707,#6708,#5960,.T.);
#8368=EDGE_CURVE('',#6708,#6707,#5961,.T.);
#8369=EDGE_CURVE('',#6707,#6709,#3783,.T.);
#8370=EDGE_CURVE('',#6709,#6709,#5962,.T.);
#8371=EDGE_CURVE('',#6710,#6710,#5963,.T.);
#8372=EDGE_CURVE('',#6711,#6711,#5964,.T.);
#8373=EDGE_CURVE('',#6712,#6712,#5965,.T.);
#8374=EDGE_CURVE('',#6713,#6713,#5966,.T.);
#8375=EDGE_CURVE('',#6714,#6714,#5967,.T.);
#8376=EDGE_CURVE('',#6715,#6715,#5968,.T.);
#8377=EDGE_CURVE('',#6716,#6716,#5969,.T.);
#8378=EDGE_CURVE('',#6717,#6718,#3784,.T.);
#8379=EDGE_CURVE('',#6717,#6719,#5970,.T.);
#8380=EDGE_CURVE('',#6720,#6719,#3785,.T.);
#8381=EDGE_CURVE('',#6718,#6720,#3786,.T.);
#8382=EDGE_CURVE('',#6721,#6721,#5971,.T.);
#8383=EDGE_CURVE('',#6721,#6708,#3787,.T.);
#8384=EDGE_CURVE('',#6722,#6723,#3788,.T.);
#8385=EDGE_CURVE('',#6723,#6717,#312,.T.);
#8386=EDGE_CURVE('',#6718,#6722,#3789,.T.);
#8387=EDGE_CURVE('',#6719,#6724,#313,.T.);
#8388=EDGE_CURVE('',#6724,#6725,#3790,.T.);
#8389=EDGE_CURVE('',#6725,#6720,#3791,.T.);
#8390=EDGE_CURVE('',#6725,#6722,#3792,.T.);
#8391=EDGE_CURVE('',#6722,#6726,#3793,.T.);
#8392=EDGE_CURVE('',#6727,#6726,#3794,.T.);
#8393=EDGE_CURVE('',#6723,#6727,#3795,.T.);
#8394=EDGE_CURVE('',#6728,#6725,#3796,.T.);
#8395=EDGE_CURVE('',#6726,#6728,#3797,.T.);
#8396=EDGE_CURVE('',#6729,#6727,#314,.T.);
#8397=EDGE_CURVE('',#6729,#6730,#5972,.T.);
#8398=EDGE_CURVE('',#6731,#6730,#315,.T.);
#8399=EDGE_CURVE('',#6731,#6724,#3798,.T.);
#8400=EDGE_CURVE('',#6728,#6731,#3799,.T.);
#8401=EDGE_CURVE('',#6732,#6729,#3800,.T.);
#8402=EDGE_CURVE('',#6726,#6732,#3801,.T.);
#8403=EDGE_CURVE('',#6730,#6733,#3802,.T.);
#8404=EDGE_CURVE('',#6733,#6728,#3803,.T.);
#8405=EDGE_CURVE('',#6733,#6732,#3804,.T.);
#8406=EDGE_CURVE('',#6734,#6734,#5973,.T.);
#8407=EDGE_CURVE('',#6735,#6735,#5974,.T.);
#8408=EDGE_CURVE('',#6736,#6736,#5975,.T.);
#8409=EDGE_CURVE('',#6737,#6737,#5976,.T.);
#8410=EDGE_CURVE('',#6738,#6738,#5977,.T.);
#8411=EDGE_CURVE('',#6739,#6739,#5978,.T.);
#8412=EDGE_CURVE('',#6740,#6740,#5979,.T.);
#8413=EDGE_CURVE('',#6741,#6741,#5980,.T.);
#8414=EDGE_CURVE('',#6741,#6742,#3805,.T.);
#8415=EDGE_CURVE('',#6742,#6742,#5981,.T.);
#8416=EDGE_CURVE('',#6716,#6743,#3806,.T.);
#8417=EDGE_CURVE('',#6743,#6743,#5982,.T.);
#8418=EDGE_CURVE('',#6740,#6744,#3807,.T.);
#8419=EDGE_CURVE('',#6744,#6744,#5983,.T.);
#8420=EDGE_CURVE('',#6715,#6745,#3808,.T.);
#8421=EDGE_CURVE('',#6745,#6745,#5984,.T.);
#8422=EDGE_CURVE('',#6739,#6746,#3809,.T.);
#8423=EDGE_CURVE('',#6746,#6746,#5985,.T.);
#8424=EDGE_CURVE('',#6714,#6747,#3810,.T.);
#8425=EDGE_CURVE('',#6747,#6747,#5986,.T.);
#8426=EDGE_CURVE('',#6738,#6748,#3811,.T.);
#8427=EDGE_CURVE('',#6748,#6748,#5987,.T.);
#8428=EDGE_CURVE('',#6713,#6749,#3812,.T.);
#8429=EDGE_CURVE('',#6749,#6749,#5988,.T.);
#8430=EDGE_CURVE('',#6737,#6750,#3813,.T.);
#8431=EDGE_CURVE('',#6750,#6750,#5989,.T.);
#8432=EDGE_CURVE('',#6712,#6751,#3814,.T.);
#8433=EDGE_CURVE('',#6751,#6751,#5990,.T.);
#8434=EDGE_CURVE('',#6736,#6752,#3815,.T.);
#8435=EDGE_CURVE('',#6752,#6752,#5991,.T.);
#8436=EDGE_CURVE('',#6711,#6753,#3816,.T.);
#8437=EDGE_CURVE('',#6753,#6753,#5992,.T.);
#8438=EDGE_CURVE('',#6735,#6754,#3817,.T.);
#8439=EDGE_CURVE('',#6754,#6754,#5993,.T.);
#8440=EDGE_CURVE('',#6710,#6755,#3818,.T.);
#8441=EDGE_CURVE('',#6755,#6755,#5994,.T.);
#8442=EDGE_CURVE('',#6734,#6721,#3819,.T.);
#8443=EDGE_CURVE('',#6756,#6757,#316,.F.);
#8444=EDGE_CURVE('',#6757,#6758,#3820,.T.);
#8445=EDGE_CURVE('',#6758,#6759,#317,.F.);
#8446=EDGE_CURVE('',#6759,#6756,#3821,.T.);
#8447=EDGE_CURVE('',#6760,#6757,#3822,.T.);
#8448=EDGE_CURVE('',#6761,#6760,#3823,.T.);
#8449=EDGE_CURVE('',#6761,#6758,#3824,.T.);
#8450=EDGE_CURVE('',#6762,#6761,#318,.F.);
#8451=EDGE_CURVE('',#6760,#6763,#319,.F.);
#8452=EDGE_CURVE('',#6763,#6762,#3825,.T.);
#8453=EDGE_CURVE('',#6764,#6765,#320,.F.);
#8454=EDGE_CURVE('',#6765,#6766,#3826,.T.);
#8455=EDGE_CURVE('',#6766,#6767,#321,.F.);
#8456=EDGE_CURVE('',#6767,#6764,#3827,.T.);
#8457=EDGE_CURVE('',#6768,#6765,#3828,.T.);
#8458=EDGE_CURVE('',#6769,#6768,#3829,.T.);
#8459=EDGE_CURVE('',#6769,#6766,#3830,.T.);
#8460=EDGE_CURVE('',#6770,#6769,#322,.F.);
#8461=EDGE_CURVE('',#6768,#6771,#323,.F.);
#8462=EDGE_CURVE('',#6771,#6770,#3831,.T.);
#8463=EDGE_CURVE('',#6772,#6773,#324,.F.);
#8464=EDGE_CURVE('',#6773,#6774,#3832,.T.);
#8465=EDGE_CURVE('',#6774,#6775,#325,.F.);
#8466=EDGE_CURVE('',#6775,#6772,#3833,.T.);
#8467=EDGE_CURVE('',#6776,#6773,#3834,.T.);
#8468=EDGE_CURVE('',#6777,#6776,#3835,.T.);
#8469=EDGE_CURVE('',#6777,#6774,#3836,.T.);
#8470=EDGE_CURVE('',#6778,#6777,#326,.F.);
#8471=EDGE_CURVE('',#6776,#6779,#327,.F.);
#8472=EDGE_CURVE('',#6779,#6778,#3837,.T.);
#8473=EDGE_CURVE('',#6780,#6781,#328,.F.);
#8474=EDGE_CURVE('',#6781,#6782,#3838,.T.);
#8475=EDGE_CURVE('',#6782,#6783,#329,.F.);
#8476=EDGE_CURVE('',#6783,#6780,#3839,.T.);
#8477=EDGE_CURVE('',#6784,#6781,#3840,.T.);
#8478=EDGE_CURVE('',#6785,#6784,#3841,.T.);
#8479=EDGE_CURVE('',#6785,#6782,#3842,.T.);
#8480=EDGE_CURVE('',#6786,#6785,#330,.F.);
#8481=EDGE_CURVE('',#6784,#6787,#331,.F.);
#8482=EDGE_CURVE('',#6787,#6786,#3843,.T.);
#8483=EDGE_CURVE('',#6787,#6778,#5995,.T.);
#8484=EDGE_CURVE('',#6775,#6780,#5996,.T.);
#8485=EDGE_CURVE('',#6779,#6786,#5997,.T.);
#8486=EDGE_CURVE('',#6783,#6772,#5998,.T.);
#8487=EDGE_CURVE('',#6771,#6762,#5999,.T.);
#8488=EDGE_CURVE('',#6759,#6764,#6000,.T.);
#8489=EDGE_CURVE('',#6763,#6770,#6001,.T.);
#8490=EDGE_CURVE('',#6767,#6756,#6002,.T.);
#8491=EDGE_CURVE('',#6788,#6788,#6003,.T.);
#8492=EDGE_CURVE('',#6788,#6789,#3844,.T.);
#8493=EDGE_CURVE('',#6789,#6789,#6004,.T.);
#8494=EDGE_CURVE('',#6790,#6790,#6005,.T.);
#8495=EDGE_CURVE('',#6791,#6791,#6006,.T.);
#8496=EDGE_CURVE('',#6791,#6790,#3845,.T.);
#8497=EDGE_CURVE('',#6792,#6793,#3846,.T.);
#8498=EDGE_CURVE('',#6793,#6794,#338,.T.);
#8499=EDGE_CURVE('',#6794,#6795,#3847,.T.);
#8500=EDGE_CURVE('',#6795,#6792,#1162,.T.);
#8501=EDGE_CURVE('',#6796,#6797,#3848,.T.);
#8502=EDGE_CURVE('',#6797,#6798,#339,.T.);
#8503=EDGE_CURVE('',#6798,#6799,#3849,.T.);
#8504=EDGE_CURVE('',#6799,#6796,#1163,.T.);
#8505=EDGE_CURVE('',#6795,#6796,#6007,.T.);
#8506=EDGE_CURVE('',#6799,#6800,#340,.T.);
#8507=EDGE_CURVE('',#6800,#6801,#6008,.T.);
#8508=EDGE_CURVE('',#6801,#6792,#341,.T.);
#8509=EDGE_CURVE('',#6801,#6802,#3850,.T.);
#8510=EDGE_CURVE('',#6803,#6802,#3851,.T.);
#8511=EDGE_CURVE('',#6804,#6803,#3852,.F.);
#8512=EDGE_CURVE('',#6805,#6804,#3853,.T.);
#8513=EDGE_CURVE('',#6793,#6805,#342,.T.);
#8514=EDGE_CURVE('',#6806,#6800,#3854,.T.);
#8515=EDGE_CURVE('',#6802,#6806,#3855,.T.);
#8516=EDGE_CURVE('',#6807,#6798,#343,.T.);
#8517=EDGE_CURVE('',#6808,#6807,#3856,.T.);
#8518=EDGE_CURVE('',#6809,#6808,#3857,.F.);
#8519=EDGE_CURVE('',#6809,#6806,#3858,.T.);
#8520=EDGE_CURVE('',#6810,#6811,#3859,.T.);
#8521=EDGE_CURVE('',#6811,#6812,#344,.T.);
#8522=EDGE_CURVE('',#6812,#6813,#3860,.T.);
#8523=EDGE_CURVE('',#6813,#6810,#1164,.T.);
#8524=EDGE_CURVE('',#6814,#6815,#3861,.T.);
#8525=EDGE_CURVE('',#6815,#6816,#345,.T.);
#8526=EDGE_CURVE('',#6816,#6817,#3862,.T.);
#8527=EDGE_CURVE('',#6817,#6814,#1165,.T.);
#8528=EDGE_CURVE('',#6813,#6814,#6009,.T.);
#8529=EDGE_CURVE('',#6817,#6818,#346,.T.);
#8530=EDGE_CURVE('',#6818,#6819,#6010,.T.);
#8531=EDGE_CURVE('',#6819,#6810,#347,.T.);
#8532=EDGE_CURVE('',#6819,#6820,#3863,.T.);
#8533=EDGE_CURVE('',#6821,#6820,#3864,.T.);
#8534=EDGE_CURVE('',#6822,#6821,#3865,.F.);
#8535=EDGE_CURVE('',#6823,#6822,#3866,.T.);
#8536=EDGE_CURVE('',#6811,#6823,#348,.T.);
#8537=EDGE_CURVE('',#6824,#6818,#3867,.T.);
#8538=EDGE_CURVE('',#6820,#6824,#3868,.T.);
#8539=EDGE_CURVE('',#6825,#6816,#349,.T.);
#8540=EDGE_CURVE('',#6826,#6825,#3869,.T.);
#8541=EDGE_CURVE('',#6827,#6826,#3870,.F.);
#8542=EDGE_CURVE('',#6827,#6824,#3871,.T.);
#8543=EDGE_CURVE('',#6828,#6829,#3872,.T.);
#8544=EDGE_CURVE('',#6829,#6830,#350,.T.);
#8545=EDGE_CURVE('',#6830,#6831,#3873,.T.);
#8546=EDGE_CURVE('',#6831,#6828,#1166,.T.);
#8547=EDGE_CURVE('',#6832,#6833,#3874,.T.);
#8548=EDGE_CURVE('',#6833,#6834,#351,.T.);
#8549=EDGE_CURVE('',#6834,#6835,#3875,.T.);
#8550=EDGE_CURVE('',#6835,#6832,#1167,.T.);
#8551=EDGE_CURVE('',#6831,#6832,#6011,.T.);
#8552=EDGE_CURVE('',#6835,#6836,#352,.T.);
#8553=EDGE_CURVE('',#6836,#6837,#6012,.T.);
#8554=EDGE_CURVE('',#6837,#6828,#353,.T.);
#8555=EDGE_CURVE('',#6837,#6838,#3876,.T.);
#8556=EDGE_CURVE('',#6839,#6838,#3877,.T.);
#8557=EDGE_CURVE('',#6840,#6839,#3878,.F.);
#8558=EDGE_CURVE('',#6841,#6840,#3879,.T.);
#8559=EDGE_CURVE('',#6829,#6841,#354,.T.);
#8560=EDGE_CURVE('',#6842,#6836,#3880,.T.);
#8561=EDGE_CURVE('',#6838,#6842,#3881,.T.);
#8562=EDGE_CURVE('',#6843,#6834,#355,.T.);
#8563=EDGE_CURVE('',#6844,#6843,#3882,.T.);
#8564=EDGE_CURVE('',#6845,#6844,#3883,.F.);
#8565=EDGE_CURVE('',#6845,#6842,#3884,.T.);
#8566=EDGE_CURVE('',#6846,#6847,#3885,.T.);
#8567=EDGE_CURVE('',#6847,#6848,#356,.T.);
#8568=EDGE_CURVE('',#6848,#6849,#3886,.T.);
#8569=EDGE_CURVE('',#6849,#6846,#1168,.T.);
#8570=EDGE_CURVE('',#6850,#6851,#3887,.T.);
#8571=EDGE_CURVE('',#6851,#6852,#357,.T.);
#8572=EDGE_CURVE('',#6852,#6853,#3888,.T.);
#8573=EDGE_CURVE('',#6853,#6850,#1169,.T.);
#8574=EDGE_CURVE('',#6849,#6850,#6013,.T.);
#8575=EDGE_CURVE('',#6853,#6854,#358,.T.);
#8576=EDGE_CURVE('',#6854,#6855,#6014,.T.);
#8577=EDGE_CURVE('',#6855,#6846,#359,.T.);
#8578=EDGE_CURVE('',#6855,#6856,#3889,.T.);
#8579=EDGE_CURVE('',#6857,#6856,#3890,.T.);
#8580=EDGE_CURVE('',#6858,#6857,#3891,.F.);
#8581=EDGE_CURVE('',#6859,#6858,#3892,.T.);
#8582=EDGE_CURVE('',#6847,#6859,#360,.T.);
#8583=EDGE_CURVE('',#6860,#6854,#3893,.T.);
#8584=EDGE_CURVE('',#6856,#6860,#3894,.T.);
#8585=EDGE_CURVE('',#6861,#6852,#361,.T.);
#8586=EDGE_CURVE('',#6862,#6861,#3895,.T.);
#8587=EDGE_CURVE('',#6863,#6862,#3896,.F.);
#8588=EDGE_CURVE('',#6863,#6860,#3897,.T.);
#8589=EDGE_CURVE('',#6864,#6865,#362,.T.);
#8590=EDGE_CURVE('',#6865,#6866,#3898,.T.);
#8591=EDGE_CURVE('',#6866,#6867,#363,.F.);
#8592=EDGE_CURVE('',#6867,#6864,#3899,.T.);
#8593=EDGE_CURVE('',#6868,#6867,#364,.F.);
#8594=EDGE_CURVE('',#6868,#6869,#3900,.T.);
#8595=EDGE_CURVE('',#6870,#6869,#3901,.T.);
#8596=EDGE_CURVE('',#6871,#6870,#3902,.F.);
#8597=EDGE_CURVE('',#6872,#6871,#3903,.T.);
#8598=EDGE_CURVE('',#6864,#6872,#365,.T.);
#8599=EDGE_CURVE('',#6873,#6874,#3904,.T.);
#8600=EDGE_CURVE('',#6874,#6875,#366,.T.);
#8601=EDGE_CURVE('',#6875,#6876,#3905,.T.);
#8602=EDGE_CURVE('',#6876,#6873,#1170,.T.);
#8603=EDGE_CURVE('',#6877,#6868,#6015,.T.);
#8604=EDGE_CURVE('',#6866,#6873,#6016,.T.);
#8605=EDGE_CURVE('',#6876,#6877,#367,.T.);
#8606=EDGE_CURVE('',#6878,#6875,#368,.T.);
#8607=EDGE_CURVE('',#6879,#6878,#3906,.T.);
#8608=EDGE_CURVE('',#6880,#6879,#3907,.F.);
#8609=EDGE_CURVE('',#6880,#6881,#3908,.T.);
#8610=EDGE_CURVE('',#6881,#6877,#3909,.T.);
#8611=EDGE_CURVE('',#6882,#6874,#6017,.T.);
#8612=EDGE_CURVE('',#6883,#6882,#369,.T.);
#8613=EDGE_CURVE('',#6883,#6884,#370,.T.);
#8614=EDGE_CURVE('',#6884,#6878,#6018,.T.);
#8615=EDGE_CURVE('',#6885,#6885,#6019,.T.);
#8616=EDGE_CURVE('',#6885,#6886,#3910,.T.);
#8617=EDGE_CURVE('',#6887,#6886,#6020,.T.);
#8618=EDGE_CURVE('',#6888,#6887,#3911,.T.);
#8619=EDGE_CURVE('',#6888,#6889,#6021,.T.);
#8620=EDGE_CURVE('',#6890,#6889,#3912,.T.);
#8621=EDGE_CURVE('',#6891,#6890,#6022,.T.);
#8622=EDGE_CURVE('',#6892,#6891,#3913,.T.);
#8623=EDGE_CURVE('',#6892,#6893,#6023,.T.);
#8624=EDGE_CURVE('',#6894,#6893,#3914,.T.);
#8625=EDGE_CURVE('',#6895,#6894,#6024,.T.);
#8626=EDGE_CURVE('',#6896,#6895,#3915,.T.);
#8627=EDGE_CURVE('',#6896,#6897,#6025,.T.);
#8628=EDGE_CURVE('',#6898,#6897,#3916,.T.);
#8629=EDGE_CURVE('',#6899,#6898,#6026,.T.);
#8630=EDGE_CURVE('',#6882,#6899,#3917,.T.);
#8631=EDGE_CURVE('',#6865,#6851,#6027,.T.);
#8632=EDGE_CURVE('',#6848,#6833,#6028,.T.);
#8633=EDGE_CURVE('',#6830,#6815,#6029,.T.);
#8634=EDGE_CURVE('',#6812,#6797,#6030,.T.);
#8635=EDGE_CURVE('',#6794,#6900,#6031,.T.);
#8636=EDGE_CURVE('',#6901,#6900,#3918,.T.);
#8637=EDGE_CURVE('',#6902,#6901,#6032,.T.);
#8638=EDGE_CURVE('',#6903,#6902,#3919,.T.);
#8639=EDGE_CURVE('',#6903,#6904,#6033,.T.);
#8640=EDGE_CURVE('',#6905,#6904,#3920,.T.);
#8641=EDGE_CURVE('',#6906,#6905,#6034,.T.);
#8642=EDGE_CURVE('',#6907,#6906,#3921,.T.);
#8643=EDGE_CURVE('',#6907,#6908,#6035,.T.);
#8644=EDGE_CURVE('',#6909,#6908,#3922,.T.);
#8645=EDGE_CURVE('',#6910,#6909,#6036,.T.);
#8646=EDGE_CURVE('',#6911,#6910,#3923,.T.);
#8647=EDGE_CURVE('',#6911,#6912,#6037,.T.);
#8648=EDGE_CURVE('',#6913,#6912,#3924,.T.);
#8649=EDGE_CURVE('',#6914,#6913,#6038,.T.);
#8650=EDGE_CURVE('',#6915,#6914,#3925,.T.);
#8651=EDGE_CURVE('',#6915,#6916,#6039,.T.);
#8652=EDGE_CURVE('',#6917,#6916,#3926,.T.);
#8653=EDGE_CURVE('',#6886,#6917,#6040,.T.);
#8654=EDGE_CURVE('',#6918,#6883,#3927,.T.);
#8655=EDGE_CURVE('',#6899,#6918,#1171,.T.);
#8656=EDGE_CURVE('',#6897,#6919,#371,.T.);
#8657=EDGE_CURVE('',#6919,#6920,#3928,.T.);
#8658=EDGE_CURVE('',#6920,#6898,#1172,.T.);
#8659=EDGE_CURVE('',#6920,#6921,#372,.T.);
#8660=EDGE_CURVE('',#6921,#6922,#6041,.T.);
#8661=EDGE_CURVE('',#6922,#6918,#373,.T.);
#8662=EDGE_CURVE('',#6922,#6923,#3929,.T.);
#8663=EDGE_CURVE('',#6924,#6923,#3930,.T.);
#8664=EDGE_CURVE('',#6925,#6924,#3931,.F.);
#8665=EDGE_CURVE('',#6884,#6925,#3932,.T.);
#8666=EDGE_CURVE('',#6926,#6921,#3933,.T.);
#8667=EDGE_CURVE('',#6923,#6926,#3934,.T.);
#8668=EDGE_CURVE('',#6927,#6919,#374,.T.);
#8669=EDGE_CURVE('',#6928,#6927,#3935,.T.);
#8670=EDGE_CURVE('',#6929,#6928,#3936,.F.);
#8671=EDGE_CURVE('',#6929,#6926,#3937,.T.);
#8672=EDGE_CURVE('',#6930,#6931,#3938,.T.);
#8673=EDGE_CURVE('',#6931,#6896,#375,.T.);
#8674=EDGE_CURVE('',#6895,#6930,#1173,.T.);
#8675=EDGE_CURVE('',#6893,#6932,#376,.T.);
#8676=EDGE_CURVE('',#6932,#6933,#3939,.T.);
#8677=EDGE_CURVE('',#6933,#6894,#1174,.T.);
#8678=EDGE_CURVE('',#6933,#6934,#377,.T.);
#8679=EDGE_CURVE('',#6934,#6935,#6042,.T.);
#8680=EDGE_CURVE('',#6935,#6930,#378,.T.);
#8681=EDGE_CURVE('',#6935,#6936,#3940,.T.);
#8682=EDGE_CURVE('',#6937,#6936,#3941,.T.);
#8683=EDGE_CURVE('',#6938,#6937,#3942,.F.);
#8684=EDGE_CURVE('',#6939,#6938,#3943,.T.);
#8685=EDGE_CURVE('',#6931,#6939,#379,.T.);
#8686=EDGE_CURVE('',#6940,#6934,#3944,.T.);
#8687=EDGE_CURVE('',#6936,#6940,#3945,.T.);
#8688=EDGE_CURVE('',#6941,#6932,#380,.T.);
#8689=EDGE_CURVE('',#6942,#6941,#3946,.T.);
#8690=EDGE_CURVE('',#6943,#6942,#3947,.F.);
#8691=EDGE_CURVE('',#6943,#6940,#3948,.T.);
#8692=EDGE_CURVE('',#6944,#6945,#3949,.F.);
#8693=EDGE_CURVE('',#6945,#6946,#3950,.T.);
#8694=EDGE_CURVE('',#6946,#6947,#3951,.F.);
#8695=EDGE_CURVE('',#6947,#6944,#3952,.T.);
#8696=EDGE_CURVE('',#6945,#6948,#3953,.T.);
#8697=EDGE_CURVE('',#6948,#6949,#3954,.T.);
#8698=EDGE_CURVE('',#6946,#6949,#3955,.T.);
#8699=EDGE_CURVE('',#6950,#6951,#3956,.F.);
#8700=EDGE_CURVE('',#6951,#6952,#3957,.T.);
#8701=EDGE_CURVE('',#6952,#6953,#3958,.F.);
#8702=EDGE_CURVE('',#6953,#6950,#3959,.T.);
#8703=EDGE_CURVE('',#6951,#6954,#3960,.T.);
#8704=EDGE_CURVE('',#6954,#6955,#3961,.T.);
#8705=EDGE_CURVE('',#6952,#6955,#3962,.T.);
#8706=EDGE_CURVE('',#6956,#6957,#3963,.F.);
#8707=EDGE_CURVE('',#6957,#6958,#3964,.T.);
#8708=EDGE_CURVE('',#6958,#6959,#3965,.F.);
#8709=EDGE_CURVE('',#6959,#6956,#3966,.T.);
#8710=EDGE_CURVE('',#6957,#6960,#3967,.T.);
#8711=EDGE_CURVE('',#6960,#6961,#3968,.T.);
#8712=EDGE_CURVE('',#6958,#6961,#3969,.T.);
#8713=EDGE_CURVE('',#6962,#6963,#3970,.F.);
#8714=EDGE_CURVE('',#6963,#6964,#3971,.T.);
#8715=EDGE_CURVE('',#6964,#6965,#3972,.F.);
#8716=EDGE_CURVE('',#6965,#6962,#3973,.T.);
#8717=EDGE_CURVE('',#6963,#6966,#3974,.T.);
#8718=EDGE_CURVE('',#6966,#6967,#3975,.T.);
#8719=EDGE_CURVE('',#6964,#6967,#3976,.T.);
#8720=EDGE_CURVE('',#6968,#6969,#3977,.F.);
#8721=EDGE_CURVE('',#6969,#6970,#3978,.T.);
#8722=EDGE_CURVE('',#6970,#6971,#3979,.F.);
#8723=EDGE_CURVE('',#6971,#6968,#3980,.T.);
#8724=EDGE_CURVE('',#6969,#6972,#3981,.T.);
#8725=EDGE_CURVE('',#6972,#6973,#3982,.T.);
#8726=EDGE_CURVE('',#6970,#6973,#3983,.T.);
#8727=EDGE_CURVE('',#6937,#6943,#3984,.T.);
#8728=EDGE_CURVE('',#6942,#6938,#3985,.T.);
#8729=EDGE_CURVE('',#6924,#6929,#3986,.T.);
#8730=EDGE_CURVE('',#6928,#6925,#3987,.T.);
#8731=EDGE_CURVE('',#6870,#6880,#3988,.T.);
#8732=EDGE_CURVE('',#6879,#6871,#3989,.T.);
#8733=EDGE_CURVE('',#6869,#6881,#3990,.T.);
#8734=EDGE_CURVE('',#6857,#6863,#3991,.T.);
#8735=EDGE_CURVE('',#6862,#6858,#3992,.T.);
#8736=EDGE_CURVE('',#6839,#6845,#3993,.T.);
#8737=EDGE_CURVE('',#6844,#6840,#3994,.T.);
#8738=EDGE_CURVE('',#6821,#6827,#3995,.T.);
#8739=EDGE_CURVE('',#6826,#6822,#3996,.T.);
#8740=EDGE_CURVE('',#6803,#6809,#3997,.T.);
#8741=EDGE_CURVE('',#6808,#6804,#3998,.T.);
#8742=EDGE_CURVE('',#6974,#6975,#3999,.T.);
#8743=EDGE_CURVE('',#6975,#6892,#381,.T.);
#8744=EDGE_CURVE('',#6891,#6974,#1175,.T.);
#8745=EDGE_CURVE('',#6889,#6976,#382,.T.);
#8746=EDGE_CURVE('',#6976,#6977,#4000,.T.);
#8747=EDGE_CURVE('',#6977,#6890,#1176,.T.);
#8748=EDGE_CURVE('',#6977,#6978,#383,.T.);
#8749=EDGE_CURVE('',#6978,#6979,#6043,.T.);
#8750=EDGE_CURVE('',#6979,#6974,#384,.T.);
#8751=EDGE_CURVE('',#6979,#6972,#4001,.T.);
#8752=EDGE_CURVE('',#6980,#6968,#4002,.T.);
#8753=EDGE_CURVE('',#6975,#6980,#385,.T.);
#8754=EDGE_CURVE('',#6973,#6978,#4003,.T.);
#8755=EDGE_CURVE('',#6981,#6976,#386,.T.);
#8756=EDGE_CURVE('',#6971,#6981,#4004,.T.);
#8757=EDGE_CURVE('',#6982,#6983,#4005,.T.);
#8758=EDGE_CURVE('',#6983,#6888,#387,.T.);
#8759=EDGE_CURVE('',#6887,#6982,#1177,.T.);
#8760=EDGE_CURVE('',#6916,#6984,#388,.T.);
#8761=EDGE_CURVE('',#6984,#6985,#4006,.T.);
#8762=EDGE_CURVE('',#6985,#6917,#1178,.T.);
#8763=EDGE_CURVE('',#6985,#6986,#389,.T.);
#8764=EDGE_CURVE('',#6986,#6987,#6044,.T.);
#8765=EDGE_CURVE('',#6987,#6982,#390,.T.);
#8766=EDGE_CURVE('',#6987,#6966,#4007,.T.);
#8767=EDGE_CURVE('',#6988,#6962,#4008,.T.);
#8768=EDGE_CURVE('',#6983,#6988,#391,.T.);
#8769=EDGE_CURVE('',#6967,#6986,#4009,.T.);
#8770=EDGE_CURVE('',#6989,#6984,#392,.T.);
#8771=EDGE_CURVE('',#6965,#6989,#4010,.T.);
#8772=EDGE_CURVE('',#6990,#6991,#4011,.T.);
#8773=EDGE_CURVE('',#6991,#6915,#393,.T.);
#8774=EDGE_CURVE('',#6914,#6990,#1179,.T.);
#8775=EDGE_CURVE('',#6912,#6992,#394,.T.);
#8776=EDGE_CURVE('',#6992,#6993,#4012,.T.);
#8777=EDGE_CURVE('',#6993,#6913,#1180,.T.);
#8778=EDGE_CURVE('',#6993,#6994,#395,.T.);
#8779=EDGE_CURVE('',#6994,#6995,#6045,.T.);
#8780=EDGE_CURVE('',#6995,#6990,#396,.T.);
#8781=EDGE_CURVE('',#6995,#6960,#4013,.T.);
#8782=EDGE_CURVE('',#6996,#6956,#4014,.T.);
#8783=EDGE_CURVE('',#6991,#6996,#397,.T.);
#8784=EDGE_CURVE('',#6961,#6994,#4015,.T.);
#8785=EDGE_CURVE('',#6997,#6992,#398,.T.);
#8786=EDGE_CURVE('',#6959,#6997,#4016,.T.);
#8787=EDGE_CURVE('',#6998,#6999,#4017,.T.);
#8788=EDGE_CURVE('',#6999,#6911,#399,.T.);
#8789=EDGE_CURVE('',#6910,#6998,#1181,.T.);
#8790=EDGE_CURVE('',#6908,#7000,#400,.T.);
#8791=EDGE_CURVE('',#7000,#7001,#4018,.T.);
#8792=EDGE_CURVE('',#7001,#6909,#1182,.T.);
#8793=EDGE_CURVE('',#7001,#7002,#401,.T.);
#8794=EDGE_CURVE('',#7002,#7003,#6046,.T.);
#8795=EDGE_CURVE('',#7003,#6998,#402,.T.);
#8796=EDGE_CURVE('',#7003,#6954,#4019,.T.);
#8797=EDGE_CURVE('',#7004,#6950,#4020,.T.);
#8798=EDGE_CURVE('',#6999,#7004,#403,.T.);
#8799=EDGE_CURVE('',#6955,#7002,#4021,.T.);
#8800=EDGE_CURVE('',#7005,#7000,#404,.T.);
#8801=EDGE_CURVE('',#6953,#7005,#4022,.T.);
#8802=EDGE_CURVE('',#7006,#7007,#4023,.T.);
#8803=EDGE_CURVE('',#7007,#6907,#405,.T.);
#8804=EDGE_CURVE('',#6906,#7006,#1183,.T.);
#8805=EDGE_CURVE('',#6904,#7008,#406,.T.);
#8806=EDGE_CURVE('',#7008,#7009,#4024,.T.);
#8807=EDGE_CURVE('',#7009,#6905,#1184,.T.);
#8808=EDGE_CURVE('',#7009,#7010,#407,.T.);
#8809=EDGE_CURVE('',#7010,#7011,#6047,.T.);
#8810=EDGE_CURVE('',#7011,#7006,#408,.T.);
#8811=EDGE_CURVE('',#6949,#7010,#4025,.T.);
#8812=EDGE_CURVE('',#7011,#6948,#4026,.T.);
#8813=EDGE_CURVE('',#7012,#7008,#409,.T.);
#8814=EDGE_CURVE('',#6947,#7012,#4027,.T.);
#8815=EDGE_CURVE('',#7013,#6903,#410,.T.);
#8816=EDGE_CURVE('',#7013,#7014,#411,.T.);
#8817=EDGE_CURVE('',#7014,#7012,#6048,.T.);
#8818=EDGE_CURVE('',#7015,#7016,#4028,.F.);
#8819=EDGE_CURVE('',#7016,#7017,#4029,.T.);
#8820=EDGE_CURVE('',#7017,#7018,#4030,.F.);
#8821=EDGE_CURVE('',#7018,#7015,#4031,.T.);
#8822=EDGE_CURVE('',#7016,#7019,#4032,.T.);
#8823=EDGE_CURVE('',#7019,#7020,#4033,.T.);
#8824=EDGE_CURVE('',#7017,#7020,#4034,.T.);
#8825=EDGE_CURVE('',#7021,#7013,#4035,.T.);
#8826=EDGE_CURVE('',#6902,#7021,#1185,.T.);
#8827=EDGE_CURVE('',#6900,#7022,#412,.T.);
#8828=EDGE_CURVE('',#7022,#7023,#4036,.T.);
#8829=EDGE_CURVE('',#7023,#6901,#1186,.T.);
#8830=EDGE_CURVE('',#7023,#7024,#413,.T.);
#8831=EDGE_CURVE('',#7024,#7025,#6049,.T.);
#8832=EDGE_CURVE('',#7025,#7021,#414,.T.);
#8833=EDGE_CURVE('',#7020,#7024,#4037,.T.);
#8834=EDGE_CURVE('',#7025,#7019,#4038,.T.);
#8835=EDGE_CURVE('',#7026,#7022,#415,.T.);
#8836=EDGE_CURVE('',#7018,#7026,#4039,.T.);
#8837=EDGE_CURVE('',#6805,#7026,#6050,.T.);
#8838=EDGE_CURVE('',#7027,#7027,#6051,.T.);
#8839=EDGE_CURVE('',#7027,#7028,#4040,.T.);
#8840=EDGE_CURVE('',#7028,#7028,#6052,.T.);
#8841=EDGE_CURVE('',#7028,#7029,#4041,.T.);
#8842=EDGE_CURVE('',#7029,#7029,#6053,.T.);
#8843=EDGE_CURVE('',#7014,#7015,#4042,.T.);
#8844=EDGE_CURVE('',#6823,#6807,#6054,.T.);
#8845=EDGE_CURVE('',#6841,#6825,#6055,.T.);
#8846=EDGE_CURVE('',#6859,#6843,#6056,.T.);
#8847=EDGE_CURVE('',#6872,#6861,#6057,.T.);
#8848=EDGE_CURVE('',#6939,#6927,#6058,.T.);
#8849=EDGE_CURVE('',#6980,#6941,#6059,.T.);
#8850=EDGE_CURVE('',#6988,#6981,#6060,.T.);
#8851=EDGE_CURVE('',#6996,#6989,#6061,.T.);
#8852=EDGE_CURVE('',#7004,#6997,#6062,.T.);
#8853=EDGE_CURVE('',#7030,#7005,#6063,.T.);
#8854=EDGE_CURVE('',#7030,#6944,#4043,.T.);
#8855=EDGE_CURVE('',#7031,#7032,#6064,.T.);
#8856=EDGE_CURVE('',#7031,#7033,#4044,.T.);
#8857=EDGE_CURVE('',#7033,#7034,#4045,.T.);
#8858=EDGE_CURVE('',#7032,#7034,#4046,.T.);
#8859=EDGE_CURVE('',#7032,#7035,#4047,.T.);
#8860=EDGE_CURVE('',#7034,#7036,#4048,.T.);
#8861=EDGE_CURVE('',#7035,#7036,#4049,.T.);
#8862=EDGE_CURVE('',#7037,#7031,#4050,.T.);
#8863=EDGE_CURVE('',#7037,#7038,#4051,.T.);
#8864=EDGE_CURVE('',#7038,#7033,#4052,.T.);
#8865=EDGE_CURVE('',#7035,#7037,#6065,.T.);
#8866=EDGE_CURVE('',#7036,#7038,#4053,.T.);
#8867=EDGE_CURVE('',#7007,#7030,#416,.T.);
#8868=EDGE_CURVE('',#7039,#7039,#6066,.T.);
#8869=EDGE_CURVE('',#7040,#7040,#6067,.T.);
#8870=EDGE_CURVE('',#7040,#7039,#4054,.T.);
#8871=EDGE_CURVE('',#7041,#7041,#6068,.T.);
#8872=EDGE_CURVE('',#7042,#7042,#6069,.T.);
#8873=EDGE_CURVE('',#7042,#7041,#4055,.T.);
#8874=EDGE_CURVE('',#7043,#7043,#6070,.T.);
#8875=EDGE_CURVE('',#7044,#7044,#6071,.T.);
#8876=EDGE_CURVE('',#7044,#7043,#4056,.T.);
#8877=EDGE_CURVE('',#7045,#7045,#6072,.T.);
#8878=EDGE_CURVE('',#7045,#7044,#4057,.T.);
#8879=EDGE_CURVE('',#7046,#7047,#4058,.T.);
#8880=EDGE_CURVE('',#7047,#7048,#4059,.T.);
#8881=EDGE_CURVE('',#7048,#7049,#4060,.T.);
#8882=EDGE_CURVE('',#7049,#7050,#4061,.T.);
#8883=EDGE_CURVE('',#7050,#7051,#4062,.T.);
#8884=EDGE_CURVE('',#7051,#7046,#4063,.T.);
#8885=EDGE_CURVE('',#7052,#7047,#4064,.T.);
#8886=EDGE_CURVE('',#7053,#7052,#4065,.T.);
#8887=EDGE_CURVE('',#7048,#7053,#4066,.T.);
#8888=EDGE_CURVE('',#7054,#7046,#4067,.T.);
#8889=EDGE_CURVE('',#7054,#7055,#4068,.T.);
#8890=EDGE_CURVE('',#7056,#7055,#4069,.T.);
#8891=EDGE_CURVE('',#7052,#7056,#4070,.T.);
#8892=EDGE_CURVE('',#7051,#7057,#4071,.T.);
#8893=EDGE_CURVE('',#7058,#7057,#4072,.T.);
#8894=EDGE_CURVE('',#7058,#7059,#4073,.T.);
#8895=EDGE_CURVE('',#7059,#7054,#4074,.T.);
#8896=EDGE_CURVE('',#7060,#7061,#4075,.T.);
#8897=EDGE_CURVE('',#7061,#7062,#4076,.T.);
#8898=EDGE_CURVE('',#7062,#7058,#4077,.T.);
#8899=EDGE_CURVE('',#7057,#7063,#4078,.T.);
#8900=EDGE_CURVE('',#7063,#7060,#4079,.T.);
#8901=EDGE_CURVE('',#7064,#7061,#4080,.T.);
#8902=EDGE_CURVE('',#7065,#7064,#4081,.T.);
#8903=EDGE_CURVE('',#7062,#7065,#4082,.T.);
#8904=EDGE_CURVE('',#7066,#7060,#4083,.T.);
#8905=EDGE_CURVE('',#7066,#7067,#4084,.T.);
#8906=EDGE_CURVE('',#7068,#7067,#4085,.T.);
#8907=EDGE_CURVE('',#7064,#7068,#4086,.T.);
#8908=EDGE_CURVE('',#7049,#7069,#4087,.T.);
#8909=EDGE_CURVE('',#7069,#7066,#4088,.T.);
#8910=EDGE_CURVE('',#7063,#7050,#4089,.T.);
#8911=EDGE_CURVE('',#7070,#7059,#4090,.T.);
#8912=EDGE_CURVE('',#7055,#7070,#4091,.T.);
#8913=EDGE_CURVE('',#7068,#7071,#4092,.T.);
#8914=EDGE_CURVE('',#7071,#7072,#4093,.T.);
#8915=EDGE_CURVE('',#7072,#7073,#4094,.T.);
#8916=EDGE_CURVE('',#7073,#7065,#4095,.T.);
#8917=EDGE_CURVE('',#7072,#7074,#4096,.T.);
#8918=EDGE_CURVE('',#7074,#7056,#4097,.T.);
#8919=EDGE_CURVE('',#7070,#7073,#4098,.T.);
#8920=EDGE_CURVE('',#7075,#7071,#4099,.T.);
#8921=EDGE_CURVE('',#7074,#7075,#4100,.T.);
#8922=EDGE_CURVE('',#7067,#7076,#4101,.T.);
#8923=EDGE_CURVE('',#7076,#7077,#4102,.T.);
#8924=EDGE_CURVE('',#7075,#7077,#4103,.T.);
#8925=EDGE_CURVE('',#7077,#7053,#4104,.T.);
#8926=EDGE_CURVE('',#7076,#7069,#4105,.T.);
#8927=EDGE_CURVE('',#7078,#7078,#6073,.T.);
#8928=EDGE_CURVE('',#7078,#7079,#4106,.T.);
#8929=EDGE_CURVE('',#7079,#7079,#6074,.T.);
#8930=EDGE_CURVE('',#7080,#7080,#6075,.T.);
#8931=EDGE_CURVE('',#7080,#7081,#4107,.T.);
#8932=EDGE_CURVE('',#7081,#7081,#6076,.T.);
#8933=EDGE_CURVE('',#7082,#7082,#6077,.T.);
#8934=EDGE_CURVE('',#7083,#7083,#6078,.T.);
#8935=EDGE_CURVE('',#7083,#7082,#4108,.T.);
#8936=EDGE_CURVE('',#7084,#7084,#6079,.T.);
#8937=EDGE_CURVE('',#7084,#7083,#4109,.T.);
#8938=EDGE_CURVE('',#7085,#7085,#6080,.T.);
#8939=EDGE_CURVE('',#7085,#7084,#4110,.T.);
#8940=EDGE_CURVE('',#7086,#7086,#6081,.T.);
#8941=EDGE_CURVE('',#7086,#7087,#4111,.T.);
#8942=EDGE_CURVE('',#7087,#7087,#6082,.T.);
#8943=EDGE_CURVE('',#7088,#7088,#6083,.T.);
#8944=EDGE_CURVE('',#7089,#7089,#6084,.T.);
#8945=EDGE_CURVE('',#7089,#7088,#4112,.T.);
#8946=EDGE_CURVE('',#7090,#7090,#6085,.T.);
#8947=EDGE_CURVE('',#7090,#7091,#4113,.T.);
#8948=EDGE_CURVE('',#7091,#7091,#6086,.T.);
#8949=EDGE_CURVE('',#7091,#7092,#4114,.T.);
#8950=EDGE_CURVE('',#7092,#7092,#6087,.T.);
#8951=EDGE_CURVE('',#7092,#7093,#4115,.T.);
#8952=EDGE_CURVE('',#7093,#7093,#6088,.T.);
#8953=EDGE_CURVE('',#7094,#7094,#6089,.T.);
#8954=EDGE_CURVE('',#7094,#7095,#4116,.T.);
#8955=EDGE_CURVE('',#7095,#7095,#6090,.T.);
#8956=EDGE_CURVE('',#7096,#7096,#6091,.T.);
#8957=EDGE_CURVE('',#7097,#7097,#6092,.T.);
#8958=EDGE_CURVE('',#7098,#7098,#6093,.T.);
#8959=EDGE_CURVE('',#7098,#7097,#4117,.T.);
#8960=EDGE_CURVE('',#7099,#7099,#6094,.T.);
#8961=EDGE_CURVE('',#7099,#7100,#4118,.T.);
#8962=EDGE_CURVE('',#7100,#7100,#6095,.T.);
#8963=EDGE_CURVE('',#7101,#7101,#6096,.T.);
#8964=EDGE_CURVE('',#7102,#7102,#6097,.T.);
#8965=EDGE_CURVE('',#7102,#7101,#4119,.T.);
#8966=EDGE_CURVE('',#7103,#7103,#6098,.T.);
#8967=EDGE_CURVE('',#7103,#7104,#4120,.T.);
#8968=EDGE_CURVE('',#7104,#7104,#6099,.T.);
#8969=EDGE_CURVE('',#7096,#7105,#4121,.T.);
#8970=EDGE_CURVE('',#7105,#7105,#6100,.T.);
#8971=EDGE_CURVE('',#7106,#7107,#6101,.T.);
#8972=EDGE_CURVE('',#7107,#7106,#6102,.T.);
#8973=EDGE_CURVE('',#7106,#7108,#4122,.T.);
#8974=EDGE_CURVE('',#7108,#7108,#6103,.T.);
#8975=EDGE_CURVE('',#7109,#7109,#6104,.T.);
#8976=EDGE_CURVE('',#7107,#7110,#4123,.T.);
#8977=EDGE_CURVE('',#7110,#7110,#6105,.T.);
#8978=EDGE_CURVE('',#7111,#7112,#6106,.T.);
#8979=EDGE_CURVE('',#7112,#7111,#6107,.T.);
#8980=EDGE_CURVE('',#7111,#7113,#4124,.T.);
#8981=EDGE_CURVE('',#7113,#7113,#6108,.T.);
#8982=EDGE_CURVE('',#7114,#7114,#6109,.T.);
#8983=EDGE_CURVE('',#7115,#7115,#6110,.T.);
#8984=EDGE_CURVE('',#7115,#7112,#4125,.T.);
#8985=EDGE_CURVE('',#7116,#7116,#6111,.T.);
#8986=EDGE_CURVE('',#7116,#7114,#4126,.T.);
#8987=EDGE_CURVE('',#7117,#7117,#6112,.T.);
#8988=EDGE_CURVE('',#7109,#7117,#4127,.T.);
#8989=EDGE_CURVE('',#7118,#7118,#6113,.T.);
#8990=EDGE_CURVE('',#7118,#7116,#4128,.T.);
#8991=EDGE_CURVE('',#7119,#7119,#6114,.T.);
#8992=EDGE_CURVE('',#7119,#7120,#4129,.T.);
#8993=EDGE_CURVE('',#7120,#7120,#6115,.T.);
#8994=EDGE_CURVE('',#7121,#7121,#6116,.T.);
#8995=EDGE_CURVE('',#7121,#7120,#4130,.T.);
#8996=EDGE_CURVE('',#7122,#7122,#6117,.T.);
#8997=EDGE_CURVE('',#7123,#7124,#6118,.T.);
#8998=EDGE_CURVE('',#7123,#7125,#4131,.T.);
#8999=EDGE_CURVE('',#7125,#7125,#6119,.T.);
#9000=EDGE_CURVE('',#7124,#7123,#6120,.T.);
#9001=EDGE_CURVE('',#7126,#7126,#6121,.T.);
#9002=EDGE_CURVE('',#7126,#7127,#4132,.T.);
#9003=EDGE_CURVE('',#7127,#7128,#6122,.T.);
#9004=EDGE_CURVE('',#7128,#7127,#6123,.T.);
#9005=EDGE_CURVE('',#7129,#7129,#6124,.T.);
#9006=EDGE_CURVE('',#7130,#7130,#6125,.T.);
#9007=EDGE_CURVE('',#7130,#7129,#4133,.T.);
#9008=EDGE_CURVE('',#7131,#7131,#6126,.T.);
#9009=EDGE_CURVE('',#7131,#7130,#4134,.T.);
#9010=EDGE_CURVE('',#7122,#7131,#4135,.T.);
#9011=EDGE_CURVE('',#7128,#7124,#6127,.T.);
#9012=EDGE_CURVE('',#7132,#7132,#6128,.T.);
#9013=EDGE_CURVE('',#7132,#7133,#4136,.T.);
#9014=EDGE_CURVE('',#7133,#7133,#6129,.T.);
#9015=EDGE_CURVE('',#7134,#7134,#6130,.T.);
#9016=EDGE_CURVE('',#7135,#7135,#6131,.T.);
#9017=EDGE_CURVE('',#7135,#7134,#4137,.T.);
#9018=EDGE_CURVE('',#7136,#7136,#6132,.T.);
#9019=EDGE_CURVE('',#7136,#7135,#4138,.T.);
#9020=EDGE_CURVE('',#7137,#7137,#6133,.T.);
#9021=EDGE_CURVE('',#7138,#7138,#6134,.T.);
#9022=EDGE_CURVE('',#7138,#7137,#4139,.T.);
#9023=EDGE_CURVE('',#7139,#7139,#6135,.T.);
#9024=EDGE_CURVE('',#7140,#7141,#6136,.T.);
#9025=EDGE_CURVE('',#7140,#7142,#6137,.T.);
#9026=EDGE_CURVE('',#7143,#7140,#6138,.T.);
#9027=EDGE_CURVE('',#7141,#7143,#6139,.T.);
#9028=EDGE_CURVE('',#7144,#7141,#6140,.T.);
#9029=EDGE_CURVE('',#7143,#7145,#4140,.T.);
#9030=EDGE_CURVE('',#7145,#7145,#6141,.T.);
#9031=EDGE_CURVE('',#7146,#7146,#6142,.T.);
#9032=EDGE_CURVE('',#7146,#7147,#4141,.T.);
#9033=EDGE_CURVE('',#7147,#7148,#6143,.T.);
#9034=EDGE_CURVE('',#7148,#7147,#6144,.T.);
#9035=EDGE_CURVE('',#7149,#7150,#6145,.T.);
#9036=EDGE_CURVE('',#7151,#7150,#6146,.T.);
#9037=EDGE_CURVE('',#7151,#7152,#6147,.T.);
#9038=EDGE_CURVE('',#7153,#7152,#6148,.T.);
#9039=EDGE_CURVE('',#7153,#7154,#6149,.T.);
#9040=EDGE_CURVE('',#7155,#7154,#6150,.T.);
#9041=EDGE_CURVE('',#7155,#7156,#6151,.T.);
#9042=EDGE_CURVE('',#7157,#7156,#6152,.T.);
#9043=EDGE_CURVE('',#7157,#7158,#6153,.T.);
#9044=EDGE_CURVE('',#7159,#7158,#6154,.T.);
#9045=EDGE_CURVE('',#7159,#7160,#6155,.T.);
#9046=EDGE_CURVE('',#7161,#7160,#6156,.T.);
#9047=EDGE_CURVE('',#7161,#7162,#6157,.T.);
#9048=EDGE_CURVE('',#7149,#7162,#6158,.T.);
#9049=EDGE_CURVE('',#7148,#7163,#4142,.T.);
#9050=EDGE_CURVE('',#7163,#7163,#6159,.T.);
#9051=EDGE_CURVE('',#7164,#7165,#6160,.T.);
#9052=EDGE_CURVE('',#7150,#7164,#4143,.T.);
#9053=EDGE_CURVE('',#7165,#7149,#4144,.T.);
#9054=EDGE_CURVE('',#7166,#7164,#6161,.T.);
#9055=EDGE_CURVE('',#7166,#7151,#4145,.T.);
#9056=EDGE_CURVE('',#7167,#7166,#6162,.T.);
#9057=EDGE_CURVE('',#7152,#7167,#4146,.T.);
#9058=EDGE_CURVE('',#7168,#7167,#6163,.T.);
#9059=EDGE_CURVE('',#7168,#7153,#4147,.T.);
#9060=EDGE_CURVE('',#7169,#7168,#6164,.T.);
#9061=EDGE_CURVE('',#7154,#7169,#4148,.T.);
#9062=EDGE_CURVE('',#7170,#7169,#6165,.T.);
#9063=EDGE_CURVE('',#7170,#7155,#4149,.T.);
#9064=EDGE_CURVE('',#7171,#7170,#6166,.T.);
#9065=EDGE_CURVE('',#7156,#7171,#4150,.T.);
#9066=EDGE_CURVE('',#7172,#7171,#6167,.T.);
#9067=EDGE_CURVE('',#7172,#7157,#4151,.T.);
#9068=EDGE_CURVE('',#7173,#7172,#6168,.T.);
#9069=EDGE_CURVE('',#7158,#7173,#4152,.T.);
#9070=EDGE_CURVE('',#7174,#7173,#6169,.T.);
#9071=EDGE_CURVE('',#7174,#7159,#4153,.T.);
#9072=EDGE_CURVE('',#7175,#7174,#6170,.T.);
#9073=EDGE_CURVE('',#7160,#7175,#4154,.T.);
#9074=EDGE_CURVE('',#7176,#7175,#6171,.T.);
#9075=EDGE_CURVE('',#7176,#7161,#4155,.T.);
#9076=EDGE_CURVE('',#7177,#7176,#6172,.T.);
#9077=EDGE_CURVE('',#7162,#7177,#4156,.T.);
#9078=EDGE_CURVE('',#7178,#7178,#6173,.T.);
#9079=EDGE_CURVE('',#7165,#7177,#6174,.T.);
#9080=EDGE_CURVE('',#7163,#7178,#4157,.T.);
#9081=EDGE_CURVE('',#7179,#7180,#4158,.T.);
#9082=EDGE_CURVE('',#7179,#7181,#1187,.T.);
#9083=EDGE_CURVE('',#7181,#7182,#6175,.T.);
#9084=EDGE_CURVE('',#7182,#7180,#1188,.T.);
#9085=EDGE_CURVE('',#7183,#7184,#4159,.T.);
#9086=EDGE_CURVE('',#7183,#7179,#1189,.T.);
#9087=EDGE_CURVE('',#7180,#7184,#1190,.T.);
#9088=EDGE_CURVE('',#7185,#7186,#4160,.T.);
#9089=EDGE_CURVE('',#7185,#7183,#1191,.T.);
#9090=EDGE_CURVE('',#7184,#7186,#1192,.T.);
#9091=EDGE_CURVE('',#7187,#7188,#4161,.T.);
#9092=EDGE_CURVE('',#7187,#7185,#1193,.T.);
#9093=EDGE_CURVE('',#7186,#7188,#1194,.T.);
#9094=EDGE_CURVE('',#7189,#7190,#4162,.T.);
#9095=EDGE_CURVE('',#7189,#7187,#1195,.T.);
#9096=EDGE_CURVE('',#7188,#7190,#1196,.T.);
#9097=EDGE_CURVE('',#7191,#7192,#4163,.T.);
#9098=EDGE_CURVE('',#7191,#7189,#1197,.T.);
#9099=EDGE_CURVE('',#7190,#7192,#1198,.T.);
#9100=EDGE_CURVE('',#7193,#7194,#4164,.T.);
#9101=EDGE_CURVE('',#7193,#7191,#1199,.T.);
#9102=EDGE_CURVE('',#7192,#7194,#1200,.T.);
#9103=EDGE_CURVE('',#7195,#7196,#4165,.T.);
#9104=EDGE_CURVE('',#7195,#7193,#1201,.T.);
#9105=EDGE_CURVE('',#7194,#7196,#1202,.T.);
#9106=EDGE_CURVE('',#7197,#7198,#4166,.T.);
#9107=EDGE_CURVE('',#7197,#7195,#1203,.T.);
#9108=EDGE_CURVE('',#7196,#7198,#1204,.T.);
#9109=EDGE_CURVE('',#7199,#7200,#4167,.T.);
#9110=EDGE_CURVE('',#7199,#7197,#1205,.T.);
#9111=EDGE_CURVE('',#7198,#7200,#1206,.T.);
#9112=EDGE_CURVE('',#7201,#7202,#4168,.T.);
#9113=EDGE_CURVE('',#7201,#7199,#1207,.T.);
#9114=EDGE_CURVE('',#7200,#7202,#1208,.T.);
#9115=EDGE_CURVE('',#7203,#7204,#4169,.T.);
#9116=EDGE_CURVE('',#7203,#7201,#1209,.T.);
#9117=EDGE_CURVE('',#7202,#7204,#1210,.T.);
#9118=EDGE_CURVE('',#7205,#7206,#4170,.T.);
#9119=EDGE_CURVE('',#7205,#7203,#1211,.T.);
#9120=EDGE_CURVE('',#7204,#7206,#1212,.T.);
#9121=EDGE_CURVE('',#7207,#7208,#4171,.T.);
#9122=EDGE_CURVE('',#7207,#7205,#1213,.T.);
#9123=EDGE_CURVE('',#7206,#7208,#1214,.T.);
#9124=EDGE_CURVE('',#7209,#7210,#4172,.T.);
#9125=EDGE_CURVE('',#7209,#7207,#1215,.T.);
#9126=EDGE_CURVE('',#7208,#7210,#1216,.T.);
#9127=EDGE_CURVE('',#7211,#7212,#4173,.T.);
#9128=EDGE_CURVE('',#7211,#7209,#1217,.T.);
#9129=EDGE_CURVE('',#7210,#7212,#1218,.T.);
#9130=EDGE_CURVE('',#7213,#7214,#4174,.T.);
#9131=EDGE_CURVE('',#7213,#7211,#1219,.T.);
#9132=EDGE_CURVE('',#7212,#7214,#1220,.T.);
#9133=EDGE_CURVE('',#7215,#7216,#4175,.T.);
#9134=EDGE_CURVE('',#7215,#7213,#1221,.T.);
#9135=EDGE_CURVE('',#7214,#7216,#1222,.T.);
#9136=EDGE_CURVE('',#7217,#7218,#4176,.T.);
#9137=EDGE_CURVE('',#7217,#7215,#1223,.T.);
#9138=EDGE_CURVE('',#7216,#7218,#1224,.T.);
#9139=EDGE_CURVE('',#7219,#7220,#4177,.T.);
#9140=EDGE_CURVE('',#7219,#7217,#1225,.T.);
#9141=EDGE_CURVE('',#7218,#7220,#1226,.T.);
#9142=EDGE_CURVE('',#7221,#7222,#4178,.T.);
#9143=EDGE_CURVE('',#7221,#7219,#1227,.T.);
#9144=EDGE_CURVE('',#7220,#7222,#1228,.T.);
#9145=EDGE_CURVE('',#7223,#7224,#4179,.T.);
#9146=EDGE_CURVE('',#7223,#7221,#1229,.T.);
#9147=EDGE_CURVE('',#7222,#7224,#1230,.T.);
#9148=EDGE_CURVE('',#7225,#7226,#4180,.T.);
#9149=EDGE_CURVE('',#7225,#7223,#1231,.T.);
#9150=EDGE_CURVE('',#7224,#7226,#1232,.T.);
#9151=EDGE_CURVE('',#7227,#7228,#4181,.T.);
#9152=EDGE_CURVE('',#7227,#7225,#1233,.T.);
#9153=EDGE_CURVE('',#7226,#7228,#1234,.T.);
#9154=EDGE_CURVE('',#7229,#7230,#4182,.T.);
#9155=EDGE_CURVE('',#7229,#7227,#1235,.T.);
#9156=EDGE_CURVE('',#7228,#7230,#1236,.T.);
#9157=EDGE_CURVE('',#7231,#7232,#4183,.T.);
#9158=EDGE_CURVE('',#7231,#7229,#1237,.T.);
#9159=EDGE_CURVE('',#7230,#7232,#1238,.T.);
#9160=EDGE_CURVE('',#7233,#7234,#4184,.T.);
#9161=EDGE_CURVE('',#7233,#7231,#1239,.T.);
#9162=EDGE_CURVE('',#7232,#7234,#1240,.T.);
#9163=EDGE_CURVE('',#7235,#7236,#4185,.T.);
#9164=EDGE_CURVE('',#7235,#7233,#1241,.T.);
#9165=EDGE_CURVE('',#7234,#7236,#1242,.T.);
#9166=EDGE_CURVE('',#7237,#7238,#4186,.T.);
#9167=EDGE_CURVE('',#7237,#7235,#1243,.T.);
#9168=EDGE_CURVE('',#7236,#7238,#1244,.T.);
#9169=EDGE_CURVE('',#7239,#7240,#4187,.T.);
#9170=EDGE_CURVE('',#7239,#7237,#1245,.T.);
#9171=EDGE_CURVE('',#7238,#7240,#1246,.T.);
#9172=EDGE_CURVE('',#7241,#7242,#4188,.T.);
#9173=EDGE_CURVE('',#7241,#7239,#1247,.T.);
#9174=EDGE_CURVE('',#7240,#7242,#1248,.T.);
#9175=EDGE_CURVE('',#7243,#7244,#4189,.T.);
#9176=EDGE_CURVE('',#7243,#7241,#1249,.T.);
#9177=EDGE_CURVE('',#7242,#7244,#1250,.T.);
#9178=EDGE_CURVE('',#7245,#7246,#4190,.T.);
#9179=EDGE_CURVE('',#7245,#7243,#1251,.T.);
#9180=EDGE_CURVE('',#7244,#7246,#1252,.T.);
#9181=EDGE_CURVE('',#7247,#7248,#4191,.T.);
#9182=EDGE_CURVE('',#7247,#7245,#1253,.T.);
#9183=EDGE_CURVE('',#7246,#7248,#1254,.T.);
#9184=EDGE_CURVE('',#7249,#7250,#4192,.T.);
#9185=EDGE_CURVE('',#7249,#7251,#1255,.T.);
#9186=EDGE_CURVE('',#7252,#7251,#6176,.T.);
#9187=EDGE_CURVE('',#7250,#7252,#1256,.T.);
#9188=EDGE_CURVE('',#7253,#7254,#4193,.T.);
#9189=EDGE_CURVE('',#7253,#7249,#1257,.T.);
#9190=EDGE_CURVE('',#7254,#7250,#1258,.T.);
#9191=EDGE_CURVE('',#7255,#7256,#4194,.T.);
#9192=EDGE_CURVE('',#7255,#7253,#1259,.T.);
#9193=EDGE_CURVE('',#7256,#7254,#1260,.T.);
#9194=EDGE_CURVE('',#7257,#7258,#4195,.T.);
#9195=EDGE_CURVE('',#7257,#7255,#1261,.T.);
#9196=EDGE_CURVE('',#7258,#7256,#1262,.T.);
#9197=EDGE_CURVE('',#7259,#7260,#4196,.T.);
#9198=EDGE_CURVE('',#7259,#7257,#1263,.T.);
#9199=EDGE_CURVE('',#7260,#7258,#1264,.T.);
#9200=EDGE_CURVE('',#7261,#7262,#4197,.T.);
#9201=EDGE_CURVE('',#7261,#7259,#1265,.T.);
#9202=EDGE_CURVE('',#7262,#7260,#1266,.T.);
#9203=EDGE_CURVE('',#7263,#7264,#4198,.T.);
#9204=EDGE_CURVE('',#7263,#7261,#1267,.T.);
#9205=EDGE_CURVE('',#7264,#7262,#1268,.T.);
#9206=EDGE_CURVE('',#7265,#7266,#4199,.T.);
#9207=EDGE_CURVE('',#7265,#7263,#1269,.T.);
#9208=EDGE_CURVE('',#7266,#7264,#1270,.T.);
#9209=EDGE_CURVE('',#7267,#7268,#4200,.T.);
#9210=EDGE_CURVE('',#7267,#7265,#1271,.T.);
#9211=EDGE_CURVE('',#7268,#7266,#1272,.T.);
#9212=EDGE_CURVE('',#7269,#7270,#4201,.T.);
#9213=EDGE_CURVE('',#7269,#7267,#1273,.T.);
#9214=EDGE_CURVE('',#7270,#7268,#1274,.T.);
#9215=EDGE_CURVE('',#7271,#7272,#4202,.T.);
#9216=EDGE_CURVE('',#7271,#7269,#1275,.T.);
#9217=EDGE_CURVE('',#7272,#7270,#1276,.T.);
#9218=EDGE_CURVE('',#7273,#7274,#4203,.T.);
#9219=EDGE_CURVE('',#7273,#7271,#1277,.T.);
#9220=EDGE_CURVE('',#7274,#7272,#1278,.T.);
#9221=EDGE_CURVE('',#7275,#7276,#4204,.T.);
#9222=EDGE_CURVE('',#7275,#7273,#1279,.T.);
#9223=EDGE_CURVE('',#7276,#7274,#1280,.T.);
#9224=EDGE_CURVE('',#7277,#7278,#4205,.T.);
#9225=EDGE_CURVE('',#7277,#7275,#1281,.T.);
#9226=EDGE_CURVE('',#7278,#7276,#1282,.T.);
#9227=EDGE_CURVE('',#7279,#7280,#4206,.T.);
#9228=EDGE_CURVE('',#7279,#7277,#1283,.T.);
#9229=EDGE_CURVE('',#7280,#7278,#1284,.T.);
#9230=EDGE_CURVE('',#7281,#7282,#4207,.T.);
#9231=EDGE_CURVE('',#7281,#7279,#1285,.T.);
#9232=EDGE_CURVE('',#7282,#7280,#1286,.T.);
#9233=EDGE_CURVE('',#7283,#7284,#4208,.T.);
#9234=EDGE_CURVE('',#7283,#7281,#1287,.T.);
#9235=EDGE_CURVE('',#7284,#7282,#1288,.T.);
#9236=EDGE_CURVE('',#7285,#7286,#4209,.T.);
#9237=EDGE_CURVE('',#7285,#7283,#1289,.T.);
#9238=EDGE_CURVE('',#7286,#7284,#1290,.T.);
#9239=EDGE_CURVE('',#7287,#7288,#4210,.T.);
#9240=EDGE_CURVE('',#7287,#7285,#1291,.T.);
#9241=EDGE_CURVE('',#7288,#7286,#1292,.T.);
#9242=EDGE_CURVE('',#7289,#7290,#4211,.T.);
#9243=EDGE_CURVE('',#7289,#7287,#1293,.T.);
#9244=EDGE_CURVE('',#7290,#7288,#1294,.T.);
#9245=EDGE_CURVE('',#7291,#7292,#4212,.T.);
#9246=EDGE_CURVE('',#7291,#7289,#1295,.T.);
#9247=EDGE_CURVE('',#7292,#7290,#1296,.T.);
#9248=EDGE_CURVE('',#7293,#7294,#4213,.T.);
#9249=EDGE_CURVE('',#7293,#7291,#1297,.T.);
#9250=EDGE_CURVE('',#7294,#7292,#1298,.T.);
#9251=EDGE_CURVE('',#7295,#7296,#4214,.T.);
#9252=EDGE_CURVE('',#7295,#7293,#1299,.T.);
#9253=EDGE_CURVE('',#7296,#7294,#1300,.T.);
#9254=EDGE_CURVE('',#7297,#7298,#4215,.T.);
#9255=EDGE_CURVE('',#7297,#7295,#1301,.T.);
#9256=EDGE_CURVE('',#7298,#7296,#1302,.T.);
#9257=EDGE_CURVE('',#7299,#7300,#4216,.T.);
#9258=EDGE_CURVE('',#7299,#7297,#1303,.T.);
#9259=EDGE_CURVE('',#7300,#7298,#1304,.T.);
#9260=EDGE_CURVE('',#7301,#7302,#4217,.T.);
#9261=EDGE_CURVE('',#7301,#7299,#1305,.T.);
#9262=EDGE_CURVE('',#7302,#7300,#1306,.T.);
#9263=EDGE_CURVE('',#7303,#7304,#4218,.T.);
#9264=EDGE_CURVE('',#7303,#7301,#1307,.T.);
#9265=EDGE_CURVE('',#7304,#7302,#1308,.T.);
#9266=EDGE_CURVE('',#7305,#7306,#4219,.T.);
#9267=EDGE_CURVE('',#7305,#7303,#1309,.T.);
#9268=EDGE_CURVE('',#7306,#7304,#1310,.T.);
#9269=EDGE_CURVE('',#7307,#7308,#4220,.T.);
#9270=EDGE_CURVE('',#7307,#7305,#1311,.T.);
#9271=EDGE_CURVE('',#7308,#7306,#1312,.T.);
#9272=EDGE_CURVE('',#7309,#7310,#4221,.T.);
#9273=EDGE_CURVE('',#7309,#7307,#1313,.T.);
#9274=EDGE_CURVE('',#7310,#7308,#1314,.T.);
#9275=EDGE_CURVE('',#7311,#7312,#4222,.T.);
#9276=EDGE_CURVE('',#7311,#7309,#1315,.T.);
#9277=EDGE_CURVE('',#7312,#7310,#1316,.T.);
#9278=EDGE_CURVE('',#7313,#7314,#4223,.T.);
#9279=EDGE_CURVE('',#7313,#7311,#1317,.T.);
#9280=EDGE_CURVE('',#7314,#7312,#1318,.T.);
#9281=EDGE_CURVE('',#7315,#7316,#4224,.T.);
#9282=EDGE_CURVE('',#7315,#7313,#1319,.T.);
#9283=EDGE_CURVE('',#7316,#7314,#1320,.T.);
#9284=EDGE_CURVE('',#7317,#7318,#4225,.T.);
#9285=EDGE_CURVE('',#7317,#7315,#1321,.T.);
#9286=EDGE_CURVE('',#7318,#7316,#1322,.T.);
#9287=EDGE_CURVE('',#7319,#7252,#1323,.T.);
#9288=EDGE_CURVE('',#7248,#7319,#1324,.T.);
#9289=EDGE_CURVE('',#7320,#7182,#1325,.T.);
#9290=EDGE_CURVE('',#7320,#7318,#1326,.T.);
#9291=EDGE_CURVE('',#7182,#7321,#6177,.T.);
#9292=EDGE_CURVE('',#7321,#7181,#6178,.T.);
#9293=EDGE_CURVE('',#7181,#7322,#1327,.T.);
#9294=EDGE_CURVE('',#7322,#7320,#6179,.T.);
#9295=EDGE_CURVE('',#7322,#7317,#1328,.T.);
#9296=EDGE_CURVE('',#7251,#7323,#1329,.T.);
#9297=EDGE_CURVE('',#7323,#7247,#1330,.T.);
#9298=EDGE_CURVE('',#7324,#7325,#4226,.T.);
#9299=EDGE_CURVE('',#7324,#7326,#4227,.T.);
#9300=EDGE_CURVE('',#7327,#7326,#4228,.T.);
#9301=EDGE_CURVE('',#7325,#7327,#4229,.T.);
#9302=EDGE_CURVE('',#7325,#7328,#6180,.T.);
#9303=EDGE_CURVE('',#7327,#7328,#4230,.T.);
#9304=EDGE_CURVE('',#7328,#7329,#4231,.T.);
#9305=EDGE_CURVE('',#7326,#7329,#4232,.T.);
#9306=EDGE_CURVE('',#7329,#7324,#6181,.T.);
#9307=EDGE_CURVE('',#7330,#7331,#4233,.T.);
#9308=EDGE_CURVE('',#7330,#7332,#4234,.T.);
#9309=EDGE_CURVE('',#7333,#7332,#4235,.T.);
#9310=EDGE_CURVE('',#7331,#7333,#4236,.T.);
#9311=EDGE_CURVE('',#7331,#7334,#6182,.T.);
#9312=EDGE_CURVE('',#7333,#7334,#4237,.T.);
#9313=EDGE_CURVE('',#7334,#7335,#4238,.T.);
#9314=EDGE_CURVE('',#7332,#7335,#4239,.T.);
#9315=EDGE_CURVE('',#7335,#7330,#6183,.T.);
#9316=EDGE_CURVE('',#7336,#7337,#4240,.T.);
#9317=EDGE_CURVE('',#7336,#7338,#4241,.T.);
#9318=EDGE_CURVE('',#7339,#7338,#4242,.T.);
#9319=EDGE_CURVE('',#7337,#7339,#4243,.T.);
#9320=EDGE_CURVE('',#7337,#7340,#6184,.T.);
#9321=EDGE_CURVE('',#7339,#7340,#4244,.T.);
#9322=EDGE_CURVE('',#7340,#7341,#4245,.T.);
#9323=EDGE_CURVE('',#7338,#7341,#4246,.T.);
#9324=EDGE_CURVE('',#7341,#7336,#6185,.T.);
#9325=EDGE_CURVE('',#7342,#7343,#4247,.T.);
#9326=EDGE_CURVE('',#7342,#7344,#4248,.T.);
#9327=EDGE_CURVE('',#7345,#7344,#4249,.T.);
#9328=EDGE_CURVE('',#7343,#7345,#4250,.T.);
#9329=EDGE_CURVE('',#7343,#7346,#6186,.T.);
#9330=EDGE_CURVE('',#7345,#7346,#4251,.T.);
#9331=EDGE_CURVE('',#7346,#7347,#4252,.T.);
#9332=EDGE_CURVE('',#7344,#7347,#4253,.T.);
#9333=EDGE_CURVE('',#7347,#7342,#6187,.T.);
#9334=EDGE_CURVE('',#7348,#7349,#4254,.T.);
#9335=EDGE_CURVE('',#7348,#7350,#4255,.T.);
#9336=EDGE_CURVE('',#7351,#7350,#4256,.T.);
#9337=EDGE_CURVE('',#7349,#7351,#4257,.T.);
#9338=EDGE_CURVE('',#7349,#7352,#6188,.T.);
#9339=EDGE_CURVE('',#7351,#7352,#4258,.T.);
#9340=EDGE_CURVE('',#7352,#7353,#4259,.T.);
#9341=EDGE_CURVE('',#7350,#7353,#4260,.T.);
#9342=EDGE_CURVE('',#7353,#7348,#6189,.T.);
#9343=EDGE_CURVE('',#7354,#7355,#4261,.T.);
#9344=EDGE_CURVE('',#7354,#7356,#4262,.T.);
#9345=EDGE_CURVE('',#7357,#7356,#4263,.T.);
#9346=EDGE_CURVE('',#7355,#7357,#4264,.T.);
#9347=EDGE_CURVE('',#7355,#7358,#6190,.T.);
#9348=EDGE_CURVE('',#7357,#7358,#4265,.T.);
#9349=EDGE_CURVE('',#7358,#7359,#4266,.T.);
#9350=EDGE_CURVE('',#7356,#7359,#4267,.T.);
#9351=EDGE_CURVE('',#7359,#7354,#6191,.T.);
#9352=EDGE_CURVE('',#7360,#7361,#4268,.T.);
#9353=EDGE_CURVE('',#7360,#7362,#4269,.T.);
#9354=EDGE_CURVE('',#7363,#7362,#4270,.T.);
#9355=EDGE_CURVE('',#7361,#7363,#4271,.T.);
#9356=EDGE_CURVE('',#7361,#7364,#6192,.T.);
#9357=EDGE_CURVE('',#7363,#7364,#4272,.T.);
#9358=EDGE_CURVE('',#7364,#7365,#4273,.T.);
#9359=EDGE_CURVE('',#7362,#7365,#4274,.T.);
#9360=EDGE_CURVE('',#7365,#7360,#6193,.T.);
#9361=EDGE_CURVE('',#7366,#7367,#4275,.T.);
#9362=EDGE_CURVE('',#7366,#7368,#4276,.T.);
#9363=EDGE_CURVE('',#7369,#7368,#4277,.T.);
#9364=EDGE_CURVE('',#7367,#7369,#4278,.T.);
#9365=EDGE_CURVE('',#7367,#7370,#6194,.T.);
#9366=EDGE_CURVE('',#7369,#7370,#4279,.T.);
#9367=EDGE_CURVE('',#7370,#7371,#4280,.T.);
#9368=EDGE_CURVE('',#7368,#7371,#4281,.T.);
#9369=EDGE_CURVE('',#7371,#7366,#6195,.T.);
#9370=EDGE_CURVE('',#7372,#7373,#4282,.T.);
#9371=EDGE_CURVE('',#7372,#7374,#4283,.T.);
#9372=EDGE_CURVE('',#7375,#7374,#4284,.T.);
#9373=EDGE_CURVE('',#7373,#7375,#4285,.T.);
#9374=EDGE_CURVE('',#7373,#7376,#6196,.T.);
#9375=EDGE_CURVE('',#7375,#7376,#4286,.T.);
#9376=EDGE_CURVE('',#7376,#7377,#4287,.T.);
#9377=EDGE_CURVE('',#7374,#7377,#4288,.T.);
#9378=EDGE_CURVE('',#7377,#7372,#6197,.T.);
#9379=EDGE_CURVE('',#7378,#7379,#4289,.T.);
#9380=EDGE_CURVE('',#7378,#7380,#4290,.T.);
#9381=EDGE_CURVE('',#7381,#7380,#4291,.T.);
#9382=EDGE_CURVE('',#7379,#7381,#4292,.T.);
#9383=EDGE_CURVE('',#7379,#7382,#6198,.T.);
#9384=EDGE_CURVE('',#7381,#7382,#4293,.T.);
#9385=EDGE_CURVE('',#7382,#7383,#4294,.T.);
#9386=EDGE_CURVE('',#7380,#7383,#4295,.T.);
#9387=EDGE_CURVE('',#7383,#7378,#6199,.T.);
#9388=EDGE_CURVE('',#7384,#7385,#4296,.T.);
#9389=EDGE_CURVE('',#7384,#7386,#4297,.T.);
#9390=EDGE_CURVE('',#7387,#7386,#4298,.T.);
#9391=EDGE_CURVE('',#7385,#7387,#4299,.T.);
#9392=EDGE_CURVE('',#7385,#7388,#6200,.T.);
#9393=EDGE_CURVE('',#7387,#7388,#4300,.T.);
#9394=EDGE_CURVE('',#7388,#7389,#4301,.T.);
#9395=EDGE_CURVE('',#7386,#7389,#4302,.T.);
#9396=EDGE_CURVE('',#7389,#7384,#6201,.T.);
#9397=EDGE_CURVE('',#7390,#7391,#4303,.T.);
#9398=EDGE_CURVE('',#7390,#7392,#4304,.T.);
#9399=EDGE_CURVE('',#7393,#7392,#4305,.T.);
#9400=EDGE_CURVE('',#7391,#7393,#4306,.T.);
#9401=EDGE_CURVE('',#7391,#7394,#6202,.T.);
#9402=EDGE_CURVE('',#7393,#7394,#4307,.T.);
#9403=EDGE_CURVE('',#7394,#7395,#4308,.T.);
#9404=EDGE_CURVE('',#7392,#7395,#4309,.T.);
#9405=EDGE_CURVE('',#7395,#7390,#6203,.T.);
#9406=EDGE_CURVE('',#7396,#7397,#4310,.T.);
#9407=EDGE_CURVE('',#7396,#7398,#4311,.T.);
#9408=EDGE_CURVE('',#7399,#7398,#4312,.T.);
#9409=EDGE_CURVE('',#7397,#7399,#4313,.T.);
#9410=EDGE_CURVE('',#7397,#7400,#6204,.T.);
#9411=EDGE_CURVE('',#7399,#7400,#4314,.T.);
#9412=EDGE_CURVE('',#7400,#7401,#4315,.T.);
#9413=EDGE_CURVE('',#7398,#7401,#4316,.T.);
#9414=EDGE_CURVE('',#7401,#7396,#6205,.T.);
#9415=EDGE_CURVE('',#7402,#7403,#4317,.T.);
#9416=EDGE_CURVE('',#7402,#7404,#4318,.T.);
#9417=EDGE_CURVE('',#7405,#7404,#4319,.T.);
#9418=EDGE_CURVE('',#7403,#7405,#4320,.T.);
#9419=EDGE_CURVE('',#7403,#7406,#6206,.T.);
#9420=EDGE_CURVE('',#7405,#7406,#4321,.T.);
#9421=EDGE_CURVE('',#7406,#7407,#4322,.T.);
#9422=EDGE_CURVE('',#7404,#7407,#4323,.T.);
#9423=EDGE_CURVE('',#7407,#7402,#6207,.T.);
#9424=EDGE_CURVE('',#7408,#7409,#4324,.T.);
#9425=EDGE_CURVE('',#7408,#7410,#4325,.T.);
#9426=EDGE_CURVE('',#7411,#7410,#4326,.T.);
#9427=EDGE_CURVE('',#7409,#7411,#4327,.T.);
#9428=EDGE_CURVE('',#7409,#7412,#6208,.T.);
#9429=EDGE_CURVE('',#7411,#7412,#4328,.T.);
#9430=EDGE_CURVE('',#7412,#7413,#4329,.T.);
#9431=EDGE_CURVE('',#7410,#7413,#4330,.T.);
#9432=EDGE_CURVE('',#7413,#7408,#6209,.T.);
#9433=EDGE_CURVE('',#7414,#7415,#4331,.T.);
#9434=EDGE_CURVE('',#7414,#7416,#4332,.T.);
#9435=EDGE_CURVE('',#7417,#7416,#4333,.T.);
#9436=EDGE_CURVE('',#7415,#7417,#4334,.T.);
#9437=EDGE_CURVE('',#7415,#7418,#6210,.T.);
#9438=EDGE_CURVE('',#7417,#7418,#4335,.T.);
#9439=EDGE_CURVE('',#7418,#7419,#4336,.T.);
#9440=EDGE_CURVE('',#7416,#7419,#4337,.T.);
#9441=EDGE_CURVE('',#7419,#7414,#6211,.T.);
#9442=EDGE_CURVE('',#7420,#7421,#4338,.T.);
#9443=EDGE_CURVE('',#7420,#7422,#4339,.T.);
#9444=EDGE_CURVE('',#7423,#7422,#4340,.T.);
#9445=EDGE_CURVE('',#7421,#7423,#4341,.T.);
#9446=EDGE_CURVE('',#7421,#7424,#6212,.T.);
#9447=EDGE_CURVE('',#7423,#7424,#4342,.T.);
#9448=EDGE_CURVE('',#7424,#7425,#4343,.T.);
#9449=EDGE_CURVE('',#7422,#7425,#4344,.T.);
#9450=EDGE_CURVE('',#7425,#7420,#6213,.T.);
#9451=EDGE_CURVE('',#7426,#7427,#4345,.T.);
#9452=EDGE_CURVE('',#7426,#7428,#4346,.T.);
#9453=EDGE_CURVE('',#7429,#7428,#4347,.T.);
#9454=EDGE_CURVE('',#7427,#7429,#4348,.T.);
#9455=EDGE_CURVE('',#7427,#7430,#6214,.T.);
#9456=EDGE_CURVE('',#7429,#7431,#4349,.T.);
#9457=EDGE_CURVE('',#7430,#7431,#6215,.T.);
#9458=EDGE_CURVE('',#7431,#7432,#4350,.T.);
#9459=EDGE_CURVE('',#7428,#7432,#4351,.T.);
#9460=EDGE_CURVE('',#7432,#7433,#6216,.T.);
#9461=EDGE_CURVE('',#7433,#7426,#6217,.T.);
#9462=EDGE_CURVE('',#7434,#7435,#4352,.T.);
#9463=EDGE_CURVE('',#7434,#7436,#4353,.T.);
#9464=EDGE_CURVE('',#7437,#7436,#4354,.T.);
#9465=EDGE_CURVE('',#7435,#7437,#4355,.T.);
#9466=EDGE_CURVE('',#7435,#7438,#6218,.T.);
#9467=EDGE_CURVE('',#7437,#7438,#4356,.T.);
#9468=EDGE_CURVE('',#7438,#7439,#4357,.T.);
#9469=EDGE_CURVE('',#7436,#7439,#4358,.T.);
#9470=EDGE_CURVE('',#7439,#7434,#6219,.T.);
#9471=EDGE_CURVE('',#7440,#7441,#4359,.T.);
#9472=EDGE_CURVE('',#7440,#7442,#4360,.T.);
#9473=EDGE_CURVE('',#7443,#7442,#4361,.T.);
#9474=EDGE_CURVE('',#7441,#7443,#4362,.T.);
#9475=EDGE_CURVE('',#7441,#7444,#6220,.T.);
#9476=EDGE_CURVE('',#7443,#7444,#4363,.T.);
#9477=EDGE_CURVE('',#7444,#7445,#4364,.T.);
#9478=EDGE_CURVE('',#7442,#7445,#4365,.T.);
#9479=EDGE_CURVE('',#7445,#7440,#6221,.T.);
#9480=EDGE_CURVE('',#7446,#7447,#4366,.T.);
#9481=EDGE_CURVE('',#7446,#7448,#4367,.T.);
#9482=EDGE_CURVE('',#7449,#7448,#4368,.T.);
#9483=EDGE_CURVE('',#7447,#7449,#4369,.T.);
#9484=EDGE_CURVE('',#7447,#7450,#6222,.T.);
#9485=EDGE_CURVE('',#7449,#7450,#4370,.T.);
#9486=EDGE_CURVE('',#7450,#7451,#4371,.T.);
#9487=EDGE_CURVE('',#7448,#7451,#4372,.T.);
#9488=EDGE_CURVE('',#7451,#7446,#6223,.T.);
#9489=EDGE_CURVE('',#7452,#7453,#4373,.T.);
#9490=EDGE_CURVE('',#7452,#7454,#4374,.T.);
#9491=EDGE_CURVE('',#7455,#7454,#4375,.T.);
#9492=EDGE_CURVE('',#7453,#7455,#4376,.T.);
#9493=EDGE_CURVE('',#7453,#7456,#6224,.T.);
#9494=EDGE_CURVE('',#7455,#7456,#4377,.T.);
#9495=EDGE_CURVE('',#7456,#7457,#4378,.T.);
#9496=EDGE_CURVE('',#7454,#7457,#4379,.T.);
#9497=EDGE_CURVE('',#7457,#7452,#6225,.T.);
#9498=EDGE_CURVE('',#7458,#7459,#4380,.T.);
#9499=EDGE_CURVE('',#7458,#7460,#4381,.T.);
#9500=EDGE_CURVE('',#7461,#7460,#4382,.T.);
#9501=EDGE_CURVE('',#7459,#7461,#4383,.T.);
#9502=EDGE_CURVE('',#7459,#7462,#6226,.T.);
#9503=EDGE_CURVE('',#7461,#7462,#4384,.T.);
#9504=EDGE_CURVE('',#7462,#7463,#4385,.T.);
#9505=EDGE_CURVE('',#7460,#7463,#4386,.T.);
#9506=EDGE_CURVE('',#7463,#7458,#6227,.T.);
#9507=EDGE_CURVE('',#7464,#7465,#4387,.T.);
#9508=EDGE_CURVE('',#7464,#7466,#4388,.T.);
#9509=EDGE_CURVE('',#7467,#7466,#4389,.T.);
#9510=EDGE_CURVE('',#7465,#7467,#4390,.T.);
#9511=EDGE_CURVE('',#7465,#7468,#6228,.T.);
#9512=EDGE_CURVE('',#7467,#7468,#4391,.T.);
#9513=EDGE_CURVE('',#7468,#7469,#4392,.T.);
#9514=EDGE_CURVE('',#7466,#7469,#4393,.T.);
#9515=EDGE_CURVE('',#7469,#7464,#6229,.T.);
#9516=EDGE_CURVE('',#7470,#7471,#4394,.T.);
#9517=EDGE_CURVE('',#7470,#7472,#4395,.T.);
#9518=EDGE_CURVE('',#7473,#7472,#4396,.T.);
#9519=EDGE_CURVE('',#7471,#7473,#4397,.T.);
#9520=EDGE_CURVE('',#7471,#7474,#6230,.T.);
#9521=EDGE_CURVE('',#7473,#7474,#4398,.T.);
#9522=EDGE_CURVE('',#7474,#7475,#4399,.T.);
#9523=EDGE_CURVE('',#7472,#7475,#4400,.T.);
#9524=EDGE_CURVE('',#7475,#7470,#6231,.T.);
#9525=EDGE_CURVE('',#7476,#7477,#4401,.T.);
#9526=EDGE_CURVE('',#7476,#7478,#4402,.T.);
#9527=EDGE_CURVE('',#7479,#7478,#4403,.T.);
#9528=EDGE_CURVE('',#7477,#7479,#4404,.T.);
#9529=EDGE_CURVE('',#7477,#7480,#6232,.T.);
#9530=EDGE_CURVE('',#7479,#7480,#4405,.T.);
#9531=EDGE_CURVE('',#7480,#7481,#4406,.T.);
#9532=EDGE_CURVE('',#7478,#7481,#4407,.T.);
#9533=EDGE_CURVE('',#7481,#7476,#6233,.T.);
#9534=EDGE_CURVE('',#7482,#7483,#4408,.T.);
#9535=EDGE_CURVE('',#7482,#7484,#4409,.T.);
#9536=EDGE_CURVE('',#7485,#7484,#4410,.T.);
#9537=EDGE_CURVE('',#7483,#7485,#4411,.T.);
#9538=EDGE_CURVE('',#7483,#7486,#6234,.T.);
#9539=EDGE_CURVE('',#7485,#7486,#4412,.T.);
#9540=EDGE_CURVE('',#7486,#7487,#4413,.T.);
#9541=EDGE_CURVE('',#7484,#7487,#4414,.T.);
#9542=EDGE_CURVE('',#7487,#7482,#6235,.T.);
#9543=EDGE_CURVE('',#7488,#7489,#4415,.T.);
#9544=EDGE_CURVE('',#7488,#7490,#4416,.T.);
#9545=EDGE_CURVE('',#7491,#7490,#4417,.T.);
#9546=EDGE_CURVE('',#7489,#7491,#4418,.T.);
#9547=EDGE_CURVE('',#7489,#7492,#6236,.T.);
#9548=EDGE_CURVE('',#7491,#7492,#4419,.T.);
#9549=EDGE_CURVE('',#7492,#7493,#4420,.T.);
#9550=EDGE_CURVE('',#7490,#7493,#4421,.T.);
#9551=EDGE_CURVE('',#7493,#7488,#6237,.T.);
#9552=EDGE_CURVE('',#7494,#7495,#4422,.T.);
#9553=EDGE_CURVE('',#7494,#7496,#4423,.T.);
#9554=EDGE_CURVE('',#7497,#7496,#4424,.T.);
#9555=EDGE_CURVE('',#7495,#7497,#4425,.T.);
#9556=EDGE_CURVE('',#7495,#7498,#6238,.T.);
#9557=EDGE_CURVE('',#7497,#7498,#4426,.T.);
#9558=EDGE_CURVE('',#7498,#7499,#4427,.T.);
#9559=EDGE_CURVE('',#7496,#7499,#4428,.T.);
#9560=EDGE_CURVE('',#7499,#7494,#6239,.T.);
#9561=EDGE_CURVE('',#7500,#7501,#4429,.T.);
#9562=EDGE_CURVE('',#7500,#7502,#4430,.T.);
#9563=EDGE_CURVE('',#7503,#7502,#4431,.T.);
#9564=EDGE_CURVE('',#7501,#7503,#4432,.T.);
#9565=EDGE_CURVE('',#7501,#7504,#6240,.T.);
#9566=EDGE_CURVE('',#7503,#7504,#4433,.T.);
#9567=EDGE_CURVE('',#7504,#7505,#4434,.T.);
#9568=EDGE_CURVE('',#7502,#7505,#4435,.T.);
#9569=EDGE_CURVE('',#7505,#7500,#6241,.T.);
#9570=EDGE_CURVE('',#7506,#7507,#4436,.T.);
#9571=EDGE_CURVE('',#7506,#7508,#4437,.T.);
#9572=EDGE_CURVE('',#7509,#7508,#4438,.T.);
#9573=EDGE_CURVE('',#7507,#7509,#4439,.T.);
#9574=EDGE_CURVE('',#7507,#7510,#6242,.T.);
#9575=EDGE_CURVE('',#7509,#7510,#4440,.T.);
#9576=EDGE_CURVE('',#7510,#7511,#4441,.T.);
#9577=EDGE_CURVE('',#7508,#7511,#4442,.T.);
#9578=EDGE_CURVE('',#7511,#7506,#6243,.T.);
#9579=EDGE_CURVE('',#7512,#7513,#4443,.T.);
#9580=EDGE_CURVE('',#7512,#7514,#4444,.T.);
#9581=EDGE_CURVE('',#7515,#7514,#4445,.T.);
#9582=EDGE_CURVE('',#7513,#7515,#4446,.T.);
#9583=EDGE_CURVE('',#7513,#7516,#6244,.T.);
#9584=EDGE_CURVE('',#7515,#7516,#4447,.T.);
#9585=EDGE_CURVE('',#7516,#7517,#4448,.T.);
#9586=EDGE_CURVE('',#7514,#7517,#4449,.T.);
#9587=EDGE_CURVE('',#7517,#7512,#6245,.T.);
#9588=EDGE_CURVE('',#7518,#7519,#4450,.T.);
#9589=EDGE_CURVE('',#7518,#7520,#4451,.T.);
#9590=EDGE_CURVE('',#7521,#7520,#4452,.T.);
#9591=EDGE_CURVE('',#7519,#7521,#4453,.T.);
#9592=EDGE_CURVE('',#7519,#7522,#6246,.T.);
#9593=EDGE_CURVE('',#7521,#7522,#4454,.T.);
#9594=EDGE_CURVE('',#7522,#7523,#4455,.T.);
#9595=EDGE_CURVE('',#7520,#7523,#4456,.T.);
#9596=EDGE_CURVE('',#7523,#7518,#6247,.T.);
#9597=EDGE_CURVE('',#7524,#7525,#4457,.T.);
#9598=EDGE_CURVE('',#7524,#7526,#4458,.T.);
#9599=EDGE_CURVE('',#7527,#7526,#4459,.T.);
#9600=EDGE_CURVE('',#7525,#7527,#4460,.T.);
#9601=EDGE_CURVE('',#7525,#7528,#6248,.T.);
#9602=EDGE_CURVE('',#7527,#7528,#4461,.T.);
#9603=EDGE_CURVE('',#7528,#7529,#4462,.T.);
#9604=EDGE_CURVE('',#7526,#7529,#4463,.T.);
#9605=EDGE_CURVE('',#7529,#7524,#6249,.T.);
#9606=EDGE_CURVE('',#7530,#7531,#4464,.T.);
#9607=EDGE_CURVE('',#7530,#7532,#4465,.T.);
#9608=EDGE_CURVE('',#7533,#7532,#4466,.T.);
#9609=EDGE_CURVE('',#7531,#7533,#4467,.T.);
#9610=EDGE_CURVE('',#7531,#7534,#6250,.T.);
#9611=EDGE_CURVE('',#7533,#7534,#4468,.T.);
#9612=EDGE_CURVE('',#7534,#7535,#4469,.T.);
#9613=EDGE_CURVE('',#7532,#7535,#4470,.T.);
#9614=EDGE_CURVE('',#7535,#7530,#6251,.T.);
#9615=EDGE_CURVE('',#7536,#7537,#4471,.T.);
#9616=EDGE_CURVE('',#7536,#7538,#4472,.T.);
#9617=EDGE_CURVE('',#7539,#7538,#4473,.T.);
#9618=EDGE_CURVE('',#7537,#7539,#4474,.T.);
#9619=EDGE_CURVE('',#7537,#7540,#6252,.T.);
#9620=EDGE_CURVE('',#7539,#7540,#4475,.T.);
#9621=EDGE_CURVE('',#7540,#7541,#4476,.T.);
#9622=EDGE_CURVE('',#7538,#7541,#4477,.T.);
#9623=EDGE_CURVE('',#7541,#7536,#6253,.T.);
#9624=EDGE_CURVE('',#7542,#7543,#4478,.T.);
#9625=EDGE_CURVE('',#7542,#7544,#4479,.T.);
#9626=EDGE_CURVE('',#7544,#7545,#4480,.T.);
#9627=EDGE_CURVE('',#7543,#7545,#4481,.T.);
#9628=EDGE_CURVE('',#7546,#7542,#4482,.T.);
#9629=EDGE_CURVE('',#7546,#7547,#4483,.T.);
#9630=EDGE_CURVE('',#7547,#7544,#4484,.T.);
#9631=EDGE_CURVE('',#7548,#7546,#4485,.T.);
#9632=EDGE_CURVE('',#7548,#7549,#4486,.T.);
#9633=EDGE_CURVE('',#7549,#7547,#4487,.T.);
#9634=EDGE_CURVE('',#7550,#7548,#4488,.T.);
#9635=EDGE_CURVE('',#7550,#7551,#4489,.T.);
#9636=EDGE_CURVE('',#7551,#7549,#4490,.T.);
#9637=EDGE_CURVE('',#7552,#7550,#4491,.T.);
#9638=EDGE_CURVE('',#7552,#7553,#4492,.T.);
#9639=EDGE_CURVE('',#7553,#7551,#4493,.T.);
#9640=EDGE_CURVE('',#7543,#7552,#4494,.T.);
#9641=EDGE_CURVE('',#7545,#7553,#4495,.T.);
#9642=EDGE_CURVE('',#7554,#7554,#6254,.T.);
#9643=EDGE_CURVE('',#7321,#7554,#4496,.T.);
#9644=EDGE_CURVE('',#7323,#7319,#6255,.T.);
#9645=EDGE_CURVE('',#7555,#7555,#6256,.T.);
#9646=EDGE_CURVE('',#7556,#7556,#6257,.T.);
#9647=EDGE_CURVE('',#7556,#7433,#4497,.T.);
#9648=EDGE_CURVE('',#7430,#7555,#4498,.T.);
#9649=EDGE_CURVE('',#7557,#7557,#6258,.T.);
#9650=EDGE_CURVE('',#7557,#7556,#4499,.T.);
#9651=EDGE_CURVE('',#7558,#7559,#4500,.T.);
#9652=EDGE_CURVE('',#7558,#7560,#1331,.T.);
#9653=EDGE_CURVE('',#7560,#7561,#6259,.T.);
#9654=EDGE_CURVE('',#7561,#7559,#1332,.T.);
#9655=EDGE_CURVE('',#7562,#7563,#4501,.T.);
#9656=EDGE_CURVE('',#7562,#7558,#1333,.T.);
#9657=EDGE_CURVE('',#7559,#7563,#1334,.T.);
#9658=EDGE_CURVE('',#7564,#7565,#4502,.T.);
#9659=EDGE_CURVE('',#7564,#7562,#1335,.T.);
#9660=EDGE_CURVE('',#7563,#7565,#1336,.T.);
#9661=EDGE_CURVE('',#7566,#7567,#4503,.T.);
#9662=EDGE_CURVE('',#7566,#7564,#1337,.T.);
#9663=EDGE_CURVE('',#7565,#7567,#1338,.T.);
#9664=EDGE_CURVE('',#7568,#7569,#4504,.T.);
#9665=EDGE_CURVE('',#7568,#7566,#1339,.T.);
#9666=EDGE_CURVE('',#7567,#7569,#1340,.T.);
#9667=EDGE_CURVE('',#7570,#7571,#4505,.T.);
#9668=EDGE_CURVE('',#7570,#7568,#1341,.T.);
#9669=EDGE_CURVE('',#7569,#7571,#1342,.T.);
#9670=EDGE_CURVE('',#7572,#7573,#4506,.T.);
#9671=EDGE_CURVE('',#7572,#7570,#1343,.T.);
#9672=EDGE_CURVE('',#7571,#7573,#1344,.T.);
#9673=EDGE_CURVE('',#7574,#7575,#4507,.T.);
#9674=EDGE_CURVE('',#7574,#7576,#1345,.T.);
#9675=EDGE_CURVE('',#7575,#7576,#6260,.T.);
#9676=EDGE_CURVE('',#7577,#7578,#4508,.T.);
#9677=EDGE_CURVE('',#7577,#7574,#1346,.T.);
#9678=EDGE_CURVE('',#7579,#7575,#6261,.T.);
#9679=EDGE_CURVE('',#7578,#7579,#1347,.T.);
#9680=EDGE_CURVE('',#7580,#7581,#4509,.T.);
#9681=EDGE_CURVE('',#7580,#7577,#1348,.T.);
#9682=EDGE_CURVE('',#7581,#7578,#1349,.T.);
#9683=EDGE_CURVE('',#7582,#7583,#4510,.T.);
#9684=EDGE_CURVE('',#7582,#7580,#1350,.T.);
#9685=EDGE_CURVE('',#7583,#7581,#1351,.T.);
#9686=EDGE_CURVE('',#7584,#7585,#4511,.T.);
#9687=EDGE_CURVE('',#7584,#7582,#1352,.T.);
#9688=EDGE_CURVE('',#7585,#7583,#1353,.T.);
#9689=EDGE_CURVE('',#7586,#7587,#4512,.T.);
#9690=EDGE_CURVE('',#7586,#7584,#1354,.T.);
#9691=EDGE_CURVE('',#7587,#7585,#1355,.T.);
#9692=EDGE_CURVE('',#7588,#7589,#4513,.T.);
#9693=EDGE_CURVE('',#7588,#7586,#1356,.T.);
#9694=EDGE_CURVE('',#7589,#7587,#1357,.T.);
#9695=EDGE_CURVE('',#7590,#7591,#4514,.T.);
#9696=EDGE_CURVE('',#7592,#7590,#4515,.T.);
#9697=EDGE_CURVE('',#7591,#7592,#4516,.T.);
#9698=EDGE_CURVE('',#7593,#7594,#4517,.T.);
#9699=EDGE_CURVE('',#7593,#7592,#4518,.T.);
#9700=EDGE_CURVE('',#7590,#7594,#4519,.T.);
#9701=EDGE_CURVE('',#7595,#7596,#4520,.T.);
#9702=EDGE_CURVE('',#7597,#7595,#4521,.T.);
#9703=EDGE_CURVE('',#7596,#7597,#4522,.T.);
#9704=EDGE_CURVE('',#7598,#7599,#4523,.T.);
#9705=EDGE_CURVE('',#7598,#7597,#4524,.T.);
#9706=EDGE_CURVE('',#7595,#7599,#4525,.T.);
#9707=EDGE_CURVE('',#7591,#7596,#4526,.T.);
#9708=EDGE_CURVE('',#7597,#7590,#4527,.T.);
#9709=EDGE_CURVE('',#7600,#7601,#4528,.T.);
#9710=EDGE_CURVE('',#7602,#7600,#4529,.T.);
#9711=EDGE_CURVE('',#7601,#7602,#4530,.T.);
#9712=EDGE_CURVE('',#7603,#7604,#4531,.T.);
#9713=EDGE_CURVE('',#7603,#7602,#4532,.T.);
#9714=EDGE_CURVE('',#7600,#7604,#4533,.T.);
#9715=EDGE_CURVE('',#7605,#7606,#4534,.T.);
#9716=EDGE_CURVE('',#7607,#7605,#4535,.T.);
#9717=EDGE_CURVE('',#7606,#7607,#4536,.T.);
#9718=EDGE_CURVE('',#7608,#7609,#4537,.T.);
#9719=EDGE_CURVE('',#7608,#7607,#4538,.T.);
#9720=EDGE_CURVE('',#7605,#7609,#4539,.T.);
#9721=EDGE_CURVE('',#7596,#7606,#4540,.T.);
#9722=EDGE_CURVE('',#7607,#7595,#4541,.T.);
#9723=EDGE_CURVE('',#7610,#7611,#4542,.T.);
#9724=EDGE_CURVE('',#7612,#7610,#4543,.T.);
#9725=EDGE_CURVE('',#7611,#7612,#4544,.T.);
#9726=EDGE_CURVE('',#7613,#7614,#4545,.T.);
#9727=EDGE_CURVE('',#7613,#7612,#4546,.T.);
#9728=EDGE_CURVE('',#7610,#7614,#4547,.T.);
#9729=EDGE_CURVE('',#7615,#7616,#4548,.T.);
#9730=EDGE_CURVE('',#7617,#7615,#4549,.T.);
#9731=EDGE_CURVE('',#7616,#7617,#4550,.T.);
#9732=EDGE_CURVE('',#7618,#7619,#4551,.T.);
#9733=EDGE_CURVE('',#7618,#7617,#4552,.T.);
#9734=EDGE_CURVE('',#7615,#7619,#4553,.T.);
#9735=EDGE_CURVE('',#7606,#7616,#4554,.T.);
#9736=EDGE_CURVE('',#7617,#7605,#4555,.T.);
#9737=EDGE_CURVE('',#7616,#7611,#4556,.T.);
#9738=EDGE_CURVE('',#7612,#7615,#4557,.T.);
#9739=EDGE_CURVE('',#7611,#7601,#4558,.T.);
#9740=EDGE_CURVE('',#7602,#7610,#4559,.T.);
#9741=EDGE_CURVE('',#7601,#7591,#4560,.T.);
#9742=EDGE_CURVE('',#7592,#7600,#4561,.T.);
#9743=EDGE_CURVE('',#7594,#7598,#4562,.T.);
#9744=EDGE_CURVE('',#7599,#7608,#4563,.T.);
#9745=EDGE_CURVE('',#7609,#7618,#4564,.T.);
#9746=EDGE_CURVE('',#7620,#7621,#4565,.T.);
#9747=EDGE_CURVE('',#7622,#7620,#4566,.T.);
#9748=EDGE_CURVE('',#7623,#7622,#4567,.T.);
#9749=EDGE_CURVE('',#7624,#7623,#4568,.T.);
#9750=EDGE_CURVE('',#7625,#7624,#4569,.T.);
#9751=EDGE_CURVE('',#7621,#7625,#4570,.T.);
#9752=EDGE_CURVE('',#7623,#7626,#4571,.T.);
#9753=EDGE_CURVE('',#7626,#7627,#4572,.T.);
#9754=EDGE_CURVE('',#7624,#7627,#4573,.T.);
#9755=EDGE_CURVE('',#7622,#7628,#4574,.T.);
#9756=EDGE_CURVE('',#7628,#7626,#4575,.T.);
#9757=EDGE_CURVE('',#7621,#7629,#4576,.T.);
#9758=EDGE_CURVE('',#7629,#7630,#4577,.T.);
#9759=EDGE_CURVE('',#7630,#7620,#4578,.T.);
#9760=EDGE_CURVE('',#7631,#7629,#4579,.T.);
#9761=EDGE_CURVE('',#7625,#7631,#4580,.T.);
#9762=EDGE_CURVE('',#7630,#7628,#4581,.T.);
#9763=EDGE_CURVE('',#7627,#7631,#4582,.T.);
#9764=EDGE_CURVE('',#7628,#7632,#4583,.T.);
#9765=EDGE_CURVE('',#7632,#7633,#4584,.T.);
#9766=EDGE_CURVE('',#7626,#7633,#4585,.T.);
#9767=EDGE_CURVE('',#7630,#7634,#4586,.T.);
#9768=EDGE_CURVE('',#7634,#7632,#4587,.T.);
#9769=EDGE_CURVE('',#7629,#7635,#4588,.T.);
#9770=EDGE_CURVE('',#7635,#7634,#4589,.T.);
#9771=EDGE_CURVE('',#7636,#7579,#1358,.T.);
#9772=EDGE_CURVE('',#7573,#7636,#1359,.T.);
#9773=EDGE_CURVE('',#7637,#7561,#1360,.T.);
#9774=EDGE_CURVE('',#7637,#7589,#1361,.T.);
#9775=EDGE_CURVE('',#7561,#7638,#6262,.T.);
#9776=EDGE_CURVE('',#7638,#7560,#6263,.T.);
#9777=EDGE_CURVE('',#7560,#7639,#1362,.T.);
#9778=EDGE_CURVE('',#7639,#7637,#6264,.T.);
#9779=EDGE_CURVE('',#7639,#7588,#1363,.T.);
#9780=EDGE_CURVE('',#7576,#7640,#1364,.T.);
#9781=EDGE_CURVE('',#7640,#7572,#1365,.T.);
#9782=EDGE_CURVE('',#7640,#7636,#6265,.F.);
#9783=EDGE_CURVE('',#7641,#7641,#6266,.T.);
#9784=EDGE_CURVE('',#7631,#7642,#4590,.T.);
#9785=EDGE_CURVE('',#7642,#7635,#4591,.T.);
#9786=EDGE_CURVE('',#7627,#7643,#4592,.T.);
#9787=EDGE_CURVE('',#7643,#7642,#4593,.T.);
#9788=EDGE_CURVE('',#7633,#7643,#4594,.T.);
#9789=EDGE_CURVE('',#7619,#7613,#4595,.T.);
#9790=EDGE_CURVE('',#7614,#7603,#4596,.T.);
#9791=EDGE_CURVE('',#7604,#7593,#4597,.T.);
#9792=EDGE_CURVE('',#7644,#7644,#6267,.T.);
#9793=EDGE_CURVE('',#7645,#7645,#6268,.T.);
#9794=EDGE_CURVE('',#7646,#7646,#6269,.T.);
#9795=EDGE_CURVE('',#7644,#7645,#4598,.T.);
#9796=EDGE_CURVE('',#7647,#7647,#6270,.T.);
#9797=EDGE_CURVE('',#7638,#7647,#4599,.T.);
#9798=EDGE_CURVE('',#7646,#7641,#4600,.T.);
#9799=ORIENTED_EDGE('',*,*,#7648,.T.);
#9800=ORIENTED_EDGE('',*,*,#7649,.T.);
#9801=ORIENTED_EDGE('',*,*,#7650,.T.);
#9802=ORIENTED_EDGE('',*,*,#7649,.F.);
#9803=ORIENTED_EDGE('',*,*,#7650,.F.);
#9804=ORIENTED_EDGE('',*,*,#7651,.T.);
#9805=ORIENTED_EDGE('',*,*,#7652,.F.);
#9806=ORIENTED_EDGE('',*,*,#7653,.F.);
#9807=ORIENTED_EDGE('',*,*,#7654,.F.);
#9808=ORIENTED_EDGE('',*,*,#7651,.F.);
#9809=ORIENTED_EDGE('',*,*,#7648,.F.);
#9810=ORIENTED_EDGE('',*,*,#7655,.T.);
#9811=ORIENTED_EDGE('',*,*,#7656,.T.);
#9812=ORIENTED_EDGE('',*,*,#7657,.T.);
#9813=ORIENTED_EDGE('',*,*,#7658,.T.);
#9814=ORIENTED_EDGE('',*,*,#7657,.F.);
#9815=ORIENTED_EDGE('',*,*,#7659,.F.);
#9816=ORIENTED_EDGE('',*,*,#7660,.F.);
#9817=ORIENTED_EDGE('',*,*,#7661,.T.);
#9818=ORIENTED_EDGE('',*,*,#7662,.F.);
#9819=ORIENTED_EDGE('',*,*,#7663,.F.);
#9820=ORIENTED_EDGE('',*,*,#7664,.F.);
#9821=ORIENTED_EDGE('',*,*,#7656,.F.);
#9822=ORIENTED_EDGE('',*,*,#7665,.F.);
#9823=ORIENTED_EDGE('',*,*,#7666,.T.);
#9824=ORIENTED_EDGE('',*,*,#7658,.F.);
#9825=ORIENTED_EDGE('',*,*,#7666,.F.);
#9826=ORIENTED_EDGE('',*,*,#7667,.T.);
#9827=ORIENTED_EDGE('',*,*,#7668,.T.);
#9828=ORIENTED_EDGE('',*,*,#7669,.T.);
#9829=ORIENTED_EDGE('',*,*,#7668,.F.);
#9830=ORIENTED_EDGE('',*,*,#7667,.F.);
#9831=ORIENTED_EDGE('',*,*,#7670,.F.);
#9832=ORIENTED_EDGE('',*,*,#7669,.F.);
#9833=ORIENTED_EDGE('',*,*,#7671,.T.);
#9834=ORIENTED_EDGE('',*,*,#7672,.F.);
#9835=ORIENTED_EDGE('',*,*,#7673,.F.);
#9836=ORIENTED_EDGE('',*,*,#7674,.F.);
#9837=ORIENTED_EDGE('',*,*,#7671,.F.);
#9838=ORIENTED_EDGE('',*,*,#7675,.T.);
#9839=ORIENTED_EDGE('',*,*,#7676,.T.);
#9840=ORIENTED_EDGE('',*,*,#7677,.T.);
#9841=ORIENTED_EDGE('',*,*,#7676,.F.);
#9842=ORIENTED_EDGE('',*,*,#7678,.F.);
#9843=ORIENTED_EDGE('',*,*,#7679,.F.);
#9844=ORIENTED_EDGE('',*,*,#7680,.F.);
#9845=ORIENTED_EDGE('',*,*,#7681,.F.);
#9846=ORIENTED_EDGE('',*,*,#7682,.T.);
#9847=ORIENTED_EDGE('',*,*,#7683,.F.);
#9848=ORIENTED_EDGE('',*,*,#7675,.F.);
#9849=ORIENTED_EDGE('',*,*,#7684,.F.);
#9850=ORIENTED_EDGE('',*,*,#7685,.T.);
#9851=ORIENTED_EDGE('',*,*,#7677,.F.);
#9852=ORIENTED_EDGE('',*,*,#7685,.F.);
#9853=ORIENTED_EDGE('',*,*,#7670,.T.);
#9854=ORIENTED_EDGE('',*,*,#7686,.T.);
#9855=ORIENTED_EDGE('',*,*,#7687,.T.);
#9856=ORIENTED_EDGE('',*,*,#7686,.F.);
#9857=ORIENTED_EDGE('',*,*,#7687,.F.);
#9858=ORIENTED_EDGE('',*,*,#7688,.T.);
#9859=ORIENTED_EDGE('',*,*,#7689,.F.);
#9860=ORIENTED_EDGE('',*,*,#7690,.T.);
#9861=ORIENTED_EDGE('',*,*,#7691,.F.);
#9862=ORIENTED_EDGE('',*,*,#7688,.F.);
#9863=ORIENTED_EDGE('',*,*,#7692,.T.);
#9864=ORIENTED_EDGE('',*,*,#7693,.T.);
#9865=ORIENTED_EDGE('',*,*,#7694,.T.);
#9866=ORIENTED_EDGE('',*,*,#7693,.F.);
#9867=ORIENTED_EDGE('',*,*,#7695,.F.);
#9868=ORIENTED_EDGE('',*,*,#7696,.F.);
#9869=ORIENTED_EDGE('',*,*,#7697,.F.);
#9870=ORIENTED_EDGE('',*,*,#7698,.F.);
#9871=ORIENTED_EDGE('',*,*,#7699,.F.);
#9872=ORIENTED_EDGE('',*,*,#7700,.F.);
#9873=ORIENTED_EDGE('',*,*,#7701,.F.);
#9874=ORIENTED_EDGE('',*,*,#7702,.F.);
#9875=ORIENTED_EDGE('',*,*,#7703,.F.);
#9876=ORIENTED_EDGE('',*,*,#7704,.F.);
#9877=ORIENTED_EDGE('',*,*,#7705,.F.);
#9878=ORIENTED_EDGE('',*,*,#7706,.F.);
#9879=ORIENTED_EDGE('',*,*,#7692,.F.);
#9880=ORIENTED_EDGE('',*,*,#7694,.F.);
#9881=ORIENTED_EDGE('',*,*,#7707,.T.);
#9882=ORIENTED_EDGE('',*,*,#7708,.T.);
#9883=ORIENTED_EDGE('',*,*,#7707,.F.);
#9884=ORIENTED_EDGE('',*,*,#7703,.T.);
#9885=ORIENTED_EDGE('',*,*,#7709,.T.);
#9886=ORIENTED_EDGE('',*,*,#7710,.T.);
#9887=ORIENTED_EDGE('',*,*,#7709,.F.);
#9888=ORIENTED_EDGE('',*,*,#7710,.F.);
#9889=ORIENTED_EDGE('',*,*,#7711,.T.);
#9890=ORIENTED_EDGE('',*,*,#7712,.T.);
#9891=ORIENTED_EDGE('',*,*,#7711,.F.);
#9892=ORIENTED_EDGE('',*,*,#7706,.T.);
#9893=ORIENTED_EDGE('',*,*,#7713,.T.);
#9894=ORIENTED_EDGE('',*,*,#7714,.T.);
#9895=ORIENTED_EDGE('',*,*,#7713,.F.);
#9896=ORIENTED_EDGE('',*,*,#7714,.F.);
#9897=ORIENTED_EDGE('',*,*,#7715,.T.);
#9898=ORIENTED_EDGE('',*,*,#7716,.T.);
#9899=ORIENTED_EDGE('',*,*,#7715,.F.);
#9900=ORIENTED_EDGE('',*,*,#7704,.T.);
#9901=ORIENTED_EDGE('',*,*,#7717,.T.);
#9902=ORIENTED_EDGE('',*,*,#7718,.T.);
#9903=ORIENTED_EDGE('',*,*,#7717,.F.);
#9904=ORIENTED_EDGE('',*,*,#7718,.F.);
#9905=ORIENTED_EDGE('',*,*,#7719,.T.);
#9906=ORIENTED_EDGE('',*,*,#7720,.T.);
#9907=ORIENTED_EDGE('',*,*,#7719,.F.);
#9908=ORIENTED_EDGE('',*,*,#7660,.T.);
#9909=ORIENTED_EDGE('',*,*,#7721,.T.);
#9910=ORIENTED_EDGE('',*,*,#7722,.T.);
#9911=ORIENTED_EDGE('',*,*,#7723,.T.);
#9912=ORIENTED_EDGE('',*,*,#7724,.T.);
#9913=ORIENTED_EDGE('',*,*,#7725,.T.);
#9914=ORIENTED_EDGE('',*,*,#7726,.T.);
#9915=ORIENTED_EDGE('',*,*,#7727,.T.);
#9916=ORIENTED_EDGE('',*,*,#7723,.F.);
#9917=ORIENTED_EDGE('',*,*,#7727,.F.);
#9918=ORIENTED_EDGE('',*,*,#7728,.F.);
#9919=ORIENTED_EDGE('',*,*,#7729,.T.);
#9920=ORIENTED_EDGE('',*,*,#7730,.F.);
#9921=ORIENTED_EDGE('',*,*,#7731,.F.);
#9922=ORIENTED_EDGE('',*,*,#7732,.F.);
#9923=ORIENTED_EDGE('',*,*,#7733,.F.);
#9924=ORIENTED_EDGE('',*,*,#7734,.F.);
#9925=ORIENTED_EDGE('',*,*,#7661,.F.);
#9926=ORIENTED_EDGE('',*,*,#7724,.F.);
#9927=ORIENTED_EDGE('',*,*,#7735,.T.);
#9928=ORIENTED_EDGE('',*,*,#7736,.T.);
#9929=ORIENTED_EDGE('',*,*,#7737,.T.);
#9930=ORIENTED_EDGE('',*,*,#7738,.T.);
#9931=ORIENTED_EDGE('',*,*,#7739,.F.);
#9932=ORIENTED_EDGE('',*,*,#7736,.F.);
#9933=ORIENTED_EDGE('',*,*,#7740,.F.);
#9934=ORIENTED_EDGE('',*,*,#7741,.F.);
#9935=ORIENTED_EDGE('',*,*,#7742,.F.);
#9936=ORIENTED_EDGE('',*,*,#7743,.F.);
#9937=ORIENTED_EDGE('',*,*,#7744,.F.);
#9938=ORIENTED_EDGE('',*,*,#7745,.T.);
#9939=ORIENTED_EDGE('',*,*,#7652,.T.);
#9940=ORIENTED_EDGE('',*,*,#7654,.T.);
#9941=ORIENTED_EDGE('',*,*,#7746,.T.);
#9942=ORIENTED_EDGE('',*,*,#7747,.F.);
#9943=ORIENTED_EDGE('',*,*,#7748,.F.);
#9944=ORIENTED_EDGE('',*,*,#7749,.T.);
#9945=ORIENTED_EDGE('',*,*,#7743,.T.);
#9946=ORIENTED_EDGE('',*,*,#7750,.T.);
#9947=ORIENTED_EDGE('',*,*,#7751,.T.);
#9948=ORIENTED_EDGE('',*,*,#7752,.T.);
#9949=ORIENTED_EDGE('',*,*,#7753,.T.);
#9950=ORIENTED_EDGE('',*,*,#7683,.T.);
#9951=ORIENTED_EDGE('',*,*,#7754,.T.);
#9952=ORIENTED_EDGE('',*,*,#7755,.T.);
#9953=ORIENTED_EDGE('',*,*,#7756,.T.);
#9954=ORIENTED_EDGE('',*,*,#7757,.T.);
#9955=ORIENTED_EDGE('',*,*,#7758,.T.);
#9956=ORIENTED_EDGE('',*,*,#7755,.F.);
#9957=ORIENTED_EDGE('',*,*,#7722,.F.);
#9958=ORIENTED_EDGE('',*,*,#7759,.F.);
#9959=ORIENTED_EDGE('',*,*,#7760,.F.);
#9960=ORIENTED_EDGE('',*,*,#7761,.F.);
#9961=ORIENTED_EDGE('',*,*,#7762,.T.);
#9962=ORIENTED_EDGE('',*,*,#7763,.F.);
#9963=ORIENTED_EDGE('',*,*,#7752,.F.);
#9964=ORIENTED_EDGE('',*,*,#7758,.F.);
#9965=ORIENTED_EDGE('',*,*,#7764,.T.);
#9966=ORIENTED_EDGE('',*,*,#7765,.F.);
#9967=ORIENTED_EDGE('',*,*,#7766,.F.);
#9968=ORIENTED_EDGE('',*,*,#7751,.F.);
#9969=ORIENTED_EDGE('',*,*,#7767,.F.);
#9970=ORIENTED_EDGE('',*,*,#7738,.F.);
#9971=ORIENTED_EDGE('',*,*,#7768,.T.);
#9972=ORIENTED_EDGE('',*,*,#7769,.F.);
#9973=ORIENTED_EDGE('',*,*,#7770,.F.);
#9974=ORIENTED_EDGE('',*,*,#7725,.F.);
#9975=ORIENTED_EDGE('',*,*,#7681,.T.);
#9976=ORIENTED_EDGE('',*,*,#7771,.T.);
#9977=ORIENTED_EDGE('',*,*,#7772,.T.);
#9978=ORIENTED_EDGE('',*,*,#7773,.T.);
#9979=ORIENTED_EDGE('',*,*,#7774,.T.);
#9980=ORIENTED_EDGE('',*,*,#7775,.T.);
#9981=ORIENTED_EDGE('',*,*,#7776,.T.);
#9982=ORIENTED_EDGE('',*,*,#7777,.T.);
#9983=ORIENTED_EDGE('',*,*,#7773,.F.);
#9984=ORIENTED_EDGE('',*,*,#7756,.F.);
#9985=ORIENTED_EDGE('',*,*,#7754,.F.);
#9986=ORIENTED_EDGE('',*,*,#7682,.F.);
#9987=ORIENTED_EDGE('',*,*,#7774,.F.);
#9988=ORIENTED_EDGE('',*,*,#7777,.F.);
#9989=ORIENTED_EDGE('',*,*,#7778,.F.);
#9990=ORIENTED_EDGE('',*,*,#7779,.T.);
#9991=ORIENTED_EDGE('',*,*,#7780,.F.);
#9992=ORIENTED_EDGE('',*,*,#7781,.F.);
#9993=ORIENTED_EDGE('',*,*,#7782,.F.);
#9994=ORIENTED_EDGE('',*,*,#7783,.T.);
#9995=ORIENTED_EDGE('',*,*,#7784,.T.);
#9996=ORIENTED_EDGE('',*,*,#7785,.T.);
#9997=ORIENTED_EDGE('',*,*,#7786,.T.);
#9998=ORIENTED_EDGE('',*,*,#7787,.F.);
#9999=ORIENTED_EDGE('',*,*,#7784,.F.);
#10000=ORIENTED_EDGE('',*,*,#7788,.F.);
#10001=ORIENTED_EDGE('',*,*,#7789,.F.);
#10002=ORIENTED_EDGE('',*,*,#7790,.F.);
#10003=ORIENTED_EDGE('',*,*,#7791,.F.);
#10004=ORIENTED_EDGE('',*,*,#7792,.F.);
#10005=ORIENTED_EDGE('',*,*,#7793,.T.);
#10006=ORIENTED_EDGE('',*,*,#7794,.F.);
#10007=ORIENTED_EDGE('',*,*,#7795,.F.);
#10008=ORIENTED_EDGE('',*,*,#7672,.T.);
#10009=ORIENTED_EDGE('',*,*,#7674,.T.);
#10010=ORIENTED_EDGE('',*,*,#7796,.F.);
#10011=ORIENTED_EDGE('',*,*,#7797,.T.);
#10012=ORIENTED_EDGE('',*,*,#7791,.T.);
#10013=ORIENTED_EDGE('',*,*,#7798,.T.);
#10014=ORIENTED_EDGE('',*,*,#7799,.T.);
#10015=ORIENTED_EDGE('',*,*,#7800,.T.);
#10016=ORIENTED_EDGE('',*,*,#7801,.T.);
#10017=ORIENTED_EDGE('',*,*,#7662,.T.);
#10018=ORIENTED_EDGE('',*,*,#7734,.T.);
#10019=ORIENTED_EDGE('',*,*,#7802,.T.);
#10020=ORIENTED_EDGE('',*,*,#7733,.T.);
#10021=ORIENTED_EDGE('',*,*,#7803,.T.);
#10022=ORIENTED_EDGE('',*,*,#7804,.T.);
#10023=ORIENTED_EDGE('',*,*,#7802,.F.);
#10024=ORIENTED_EDGE('',*,*,#7772,.F.);
#10025=ORIENTED_EDGE('',*,*,#7805,.F.);
#10026=ORIENTED_EDGE('',*,*,#7806,.F.);
#10027=ORIENTED_EDGE('',*,*,#7807,.F.);
#10028=ORIENTED_EDGE('',*,*,#7808,.T.);
#10029=ORIENTED_EDGE('',*,*,#7809,.F.);
#10030=ORIENTED_EDGE('',*,*,#7800,.F.);
#10031=ORIENTED_EDGE('',*,*,#7804,.F.);
#10032=ORIENTED_EDGE('',*,*,#7810,.T.);
#10033=ORIENTED_EDGE('',*,*,#7811,.F.);
#10034=ORIENTED_EDGE('',*,*,#7812,.F.);
#10035=ORIENTED_EDGE('',*,*,#7799,.F.);
#10036=ORIENTED_EDGE('',*,*,#7813,.F.);
#10037=ORIENTED_EDGE('',*,*,#7786,.F.);
#10038=ORIENTED_EDGE('',*,*,#7814,.T.);
#10039=ORIENTED_EDGE('',*,*,#7815,.F.);
#10040=ORIENTED_EDGE('',*,*,#7816,.F.);
#10041=ORIENTED_EDGE('',*,*,#7775,.F.);
#10042=ORIENTED_EDGE('',*,*,#7817,.T.);
#10043=ORIENTED_EDGE('',*,*,#7818,.T.);
#10044=ORIENTED_EDGE('',*,*,#7684,.T.);
#10045=ORIENTED_EDGE('',*,*,#7818,.F.);
#10046=ORIENTED_EDGE('',*,*,#7819,.F.);
#10047=ORIENTED_EDGE('',*,*,#7820,.F.);
#10048=ORIENTED_EDGE('',*,*,#7821,.F.);
#10049=ORIENTED_EDGE('',*,*,#7822,.F.);
#10050=ORIENTED_EDGE('',*,*,#7823,.F.);
#10051=ORIENTED_EDGE('',*,*,#7824,.F.);
#10052=ORIENTED_EDGE('',*,*,#7825,.F.);
#10053=ORIENTED_EDGE('',*,*,#7826,.F.);
#10054=ORIENTED_EDGE('',*,*,#7827,.F.);
#10055=ORIENTED_EDGE('',*,*,#7828,.T.);
#10056=ORIENTED_EDGE('',*,*,#7817,.F.);
#10057=ORIENTED_EDGE('',*,*,#7827,.T.);
#10058=ORIENTED_EDGE('',*,*,#7829,.T.);
#10059=ORIENTED_EDGE('',*,*,#7665,.T.);
#10060=ORIENTED_EDGE('',*,*,#7829,.F.);
#10061=ORIENTED_EDGE('',*,*,#7807,.T.);
#10062=ORIENTED_EDGE('',*,*,#7830,.T.);
#10063=ORIENTED_EDGE('',*,*,#7823,.T.);
#10064=ORIENTED_EDGE('',*,*,#7831,.T.);
#10065=ORIENTED_EDGE('',*,*,#7822,.T.);
#10066=ORIENTED_EDGE('',*,*,#7832,.T.);
#10067=ORIENTED_EDGE('',*,*,#7833,.T.);
#10068=ORIENTED_EDGE('',*,*,#7831,.F.);
#10069=ORIENTED_EDGE('',*,*,#7834,.T.);
#10070=ORIENTED_EDGE('',*,*,#7835,.T.);
#10071=ORIENTED_EDGE('',*,*,#7832,.F.);
#10072=ORIENTED_EDGE('',*,*,#7821,.T.);
#10073=ORIENTED_EDGE('',*,*,#7836,.T.);
#10074=ORIENTED_EDGE('',*,*,#7837,.T.);
#10075=ORIENTED_EDGE('',*,*,#7834,.F.);
#10076=ORIENTED_EDGE('',*,*,#7820,.T.);
#10077=ORIENTED_EDGE('',*,*,#7761,.T.);
#10078=ORIENTED_EDGE('',*,*,#7836,.F.);
#10079=ORIENTED_EDGE('',*,*,#7819,.T.);
#10080=ORIENTED_EDGE('',*,*,#7838,.T.);
#10081=ORIENTED_EDGE('',*,*,#7839,.T.);
#10082=ORIENTED_EDGE('',*,*,#7825,.T.);
#10083=ORIENTED_EDGE('',*,*,#7840,.T.);
#10084=ORIENTED_EDGE('',*,*,#7841,.T.);
#10085=ORIENTED_EDGE('',*,*,#7842,.T.);
#10086=ORIENTED_EDGE('',*,*,#7840,.F.);
#10087=ORIENTED_EDGE('',*,*,#7824,.T.);
#10088=ORIENTED_EDGE('',*,*,#7830,.F.);
#10089=ORIENTED_EDGE('',*,*,#7826,.T.);
#10090=ORIENTED_EDGE('',*,*,#7839,.F.);
#10091=ORIENTED_EDGE('',*,*,#7843,.T.);
#10092=ORIENTED_EDGE('',*,*,#7838,.F.);
#10093=ORIENTED_EDGE('',*,*,#7841,.F.);
#10094=ORIENTED_EDGE('',*,*,#7844,.T.);
#10095=ORIENTED_EDGE('',*,*,#7845,.F.);
#10096=ORIENTED_EDGE('',*,*,#7846,.F.);
#10097=ORIENTED_EDGE('',*,*,#7842,.F.);
#10098=ORIENTED_EDGE('',*,*,#7806,.T.);
#10099=ORIENTED_EDGE('',*,*,#7847,.F.);
#10100=ORIENTED_EDGE('',*,*,#7844,.F.);
#10101=ORIENTED_EDGE('',*,*,#7788,.T.);
#10102=ORIENTED_EDGE('',*,*,#7783,.F.);
#10103=ORIENTED_EDGE('',*,*,#7813,.T.);
#10104=ORIENTED_EDGE('',*,*,#7798,.F.);
#10105=ORIENTED_EDGE('',*,*,#7790,.T.);
#10106=ORIENTED_EDGE('',*,*,#7848,.T.);
#10107=ORIENTED_EDGE('',*,*,#7849,.T.);
#10108=ORIENTED_EDGE('',*,*,#7663,.T.);
#10109=ORIENTED_EDGE('',*,*,#7801,.F.);
#10110=ORIENTED_EDGE('',*,*,#7809,.T.);
#10111=ORIENTED_EDGE('',*,*,#7850,.T.);
#10112=ORIENTED_EDGE('',*,*,#7851,.T.);
#10113=ORIENTED_EDGE('',*,*,#7664,.T.);
#10114=ORIENTED_EDGE('',*,*,#7849,.F.);
#10115=ORIENTED_EDGE('',*,*,#7852,.T.);
#10116=ORIENTED_EDGE('',*,*,#7759,.T.);
#10117=ORIENTED_EDGE('',*,*,#7721,.F.);
#10118=ORIENTED_EDGE('',*,*,#7659,.T.);
#10119=ORIENTED_EDGE('',*,*,#7851,.F.);
#10120=ORIENTED_EDGE('',*,*,#7853,.T.);
#10121=ORIENTED_EDGE('',*,*,#7837,.F.);
#10122=ORIENTED_EDGE('',*,*,#7760,.T.);
#10123=ORIENTED_EDGE('',*,*,#7853,.F.);
#10124=ORIENTED_EDGE('',*,*,#7854,.F.);
#10125=ORIENTED_EDGE('',*,*,#7835,.F.);
#10126=ORIENTED_EDGE('',*,*,#7854,.T.);
#10127=ORIENTED_EDGE('',*,*,#7852,.F.);
#10128=ORIENTED_EDGE('',*,*,#7855,.F.);
#10129=ORIENTED_EDGE('',*,*,#7833,.F.);
#10130=ORIENTED_EDGE('',*,*,#7855,.T.);
#10131=ORIENTED_EDGE('',*,*,#7850,.F.);
#10132=ORIENTED_EDGE('',*,*,#7808,.F.);
#10133=ORIENTED_EDGE('',*,*,#7740,.T.);
#10134=ORIENTED_EDGE('',*,*,#7735,.F.);
#10135=ORIENTED_EDGE('',*,*,#7767,.T.);
#10136=ORIENTED_EDGE('',*,*,#7750,.F.);
#10137=ORIENTED_EDGE('',*,*,#7742,.T.);
#10138=ORIENTED_EDGE('',*,*,#7856,.T.);
#10139=ORIENTED_EDGE('',*,*,#7857,.T.);
#10140=ORIENTED_EDGE('',*,*,#7678,.T.);
#10141=ORIENTED_EDGE('',*,*,#7753,.F.);
#10142=ORIENTED_EDGE('',*,*,#7763,.T.);
#10143=ORIENTED_EDGE('',*,*,#7858,.T.);
#10144=ORIENTED_EDGE('',*,*,#7859,.T.);
#10145=ORIENTED_EDGE('',*,*,#7679,.T.);
#10146=ORIENTED_EDGE('',*,*,#7857,.F.);
#10147=ORIENTED_EDGE('',*,*,#7845,.T.);
#10148=ORIENTED_EDGE('',*,*,#7805,.T.);
#10149=ORIENTED_EDGE('',*,*,#7771,.F.);
#10150=ORIENTED_EDGE('',*,*,#7680,.T.);
#10151=ORIENTED_EDGE('',*,*,#7859,.F.);
#10152=ORIENTED_EDGE('',*,*,#7847,.T.);
#10153=ORIENTED_EDGE('',*,*,#7843,.F.);
#10154=ORIENTED_EDGE('',*,*,#7846,.T.);
#10155=ORIENTED_EDGE('',*,*,#7858,.F.);
#10156=ORIENTED_EDGE('',*,*,#7762,.F.);
#10157=ORIENTED_EDGE('',*,*,#7860,.T.);
#10158=ORIENTED_EDGE('',*,*,#7861,.T.);
#10159=ORIENTED_EDGE('',*,*,#7862,.T.);
#10160=ORIENTED_EDGE('',*,*,#7861,.F.);
#10161=ORIENTED_EDGE('',*,*,#7828,.F.);
#10162=ORIENTED_EDGE('',*,*,#7863,.T.);
#10163=ORIENTED_EDGE('',*,*,#7860,.F.);
#10164=ORIENTED_EDGE('',*,*,#7863,.F.);
#10165=ORIENTED_EDGE('',*,*,#7812,.T.);
#10166=ORIENTED_EDGE('',*,*,#7864,.T.);
#10167=ORIENTED_EDGE('',*,*,#7865,.T.);
#10168=ORIENTED_EDGE('',*,*,#7792,.T.);
#10169=ORIENTED_EDGE('',*,*,#7797,.F.);
#10170=ORIENTED_EDGE('',*,*,#7866,.T.);
#10171=ORIENTED_EDGE('',*,*,#7867,.T.);
#10172=ORIENTED_EDGE('',*,*,#7865,.F.);
#10173=ORIENTED_EDGE('',*,*,#7868,.T.);
#10174=ORIENTED_EDGE('',*,*,#7732,.T.);
#10175=ORIENTED_EDGE('',*,*,#7866,.F.);
#10176=ORIENTED_EDGE('',*,*,#7869,.T.);
#10177=ORIENTED_EDGE('',*,*,#7810,.F.);
#10178=ORIENTED_EDGE('',*,*,#7803,.F.);
#10179=ORIENTED_EDGE('',*,*,#7869,.F.);
#10180=ORIENTED_EDGE('',*,*,#7868,.F.);
#10181=ORIENTED_EDGE('',*,*,#7864,.F.);
#10182=ORIENTED_EDGE('',*,*,#7811,.T.);
#10183=ORIENTED_EDGE('',*,*,#7870,.T.);
#10184=ORIENTED_EDGE('',*,*,#7871,.T.);
#10185=ORIENTED_EDGE('',*,*,#7872,.T.);
#10186=ORIENTED_EDGE('',*,*,#7873,.T.);
#10187=ORIENTED_EDGE('',*,*,#7787,.T.);
#10188=ORIENTED_EDGE('',*,*,#7872,.F.);
#10189=ORIENTED_EDGE('',*,*,#7874,.T.);
#10190=ORIENTED_EDGE('',*,*,#7814,.F.);
#10191=ORIENTED_EDGE('',*,*,#7785,.F.);
#10192=ORIENTED_EDGE('',*,*,#7816,.T.);
#10193=ORIENTED_EDGE('',*,*,#7875,.T.);
#10194=ORIENTED_EDGE('',*,*,#7870,.F.);
#10195=ORIENTED_EDGE('',*,*,#7778,.T.);
#10196=ORIENTED_EDGE('',*,*,#7776,.F.);
#10197=ORIENTED_EDGE('',*,*,#7874,.F.);
#10198=ORIENTED_EDGE('',*,*,#7871,.F.);
#10199=ORIENTED_EDGE('',*,*,#7875,.F.);
#10200=ORIENTED_EDGE('',*,*,#7815,.T.);
#10201=ORIENTED_EDGE('',*,*,#7766,.T.);
#10202=ORIENTED_EDGE('',*,*,#7876,.T.);
#10203=ORIENTED_EDGE('',*,*,#7877,.T.);
#10204=ORIENTED_EDGE('',*,*,#7744,.T.);
#10205=ORIENTED_EDGE('',*,*,#7749,.F.);
#10206=ORIENTED_EDGE('',*,*,#7878,.T.);
#10207=ORIENTED_EDGE('',*,*,#7879,.T.);
#10208=ORIENTED_EDGE('',*,*,#7877,.F.);
#10209=ORIENTED_EDGE('',*,*,#7880,.T.);
#10210=ORIENTED_EDGE('',*,*,#7782,.T.);
#10211=ORIENTED_EDGE('',*,*,#7878,.F.);
#10212=ORIENTED_EDGE('',*,*,#7881,.T.);
#10213=ORIENTED_EDGE('',*,*,#7764,.F.);
#10214=ORIENTED_EDGE('',*,*,#7757,.F.);
#10215=ORIENTED_EDGE('',*,*,#7881,.F.);
#10216=ORIENTED_EDGE('',*,*,#7880,.F.);
#10217=ORIENTED_EDGE('',*,*,#7876,.F.);
#10218=ORIENTED_EDGE('',*,*,#7765,.T.);
#10219=ORIENTED_EDGE('',*,*,#7770,.T.);
#10220=ORIENTED_EDGE('',*,*,#7882,.T.);
#10221=ORIENTED_EDGE('',*,*,#7883,.T.);
#10222=ORIENTED_EDGE('',*,*,#7728,.T.);
#10223=ORIENTED_EDGE('',*,*,#7726,.F.);
#10224=ORIENTED_EDGE('',*,*,#7884,.T.);
#10225=ORIENTED_EDGE('',*,*,#7885,.T.);
#10226=ORIENTED_EDGE('',*,*,#7883,.F.);
#10227=ORIENTED_EDGE('',*,*,#7886,.T.);
#10228=ORIENTED_EDGE('',*,*,#7739,.T.);
#10229=ORIENTED_EDGE('',*,*,#7884,.F.);
#10230=ORIENTED_EDGE('',*,*,#7887,.T.);
#10231=ORIENTED_EDGE('',*,*,#7768,.F.);
#10232=ORIENTED_EDGE('',*,*,#7737,.F.);
#10233=ORIENTED_EDGE('',*,*,#7887,.F.);
#10234=ORIENTED_EDGE('',*,*,#7886,.F.);
#10235=ORIENTED_EDGE('',*,*,#7882,.F.);
#10236=ORIENTED_EDGE('',*,*,#7769,.T.);
#10237=ORIENTED_EDGE('',*,*,#7888,.T.);
#10238=ORIENTED_EDGE('',*,*,#7747,.T.);
#10239=ORIENTED_EDGE('',*,*,#7889,.T.);
#10240=ORIENTED_EDGE('',*,*,#7695,.T.);
#10241=ORIENTED_EDGE('',*,*,#7890,.T.);
#10242=ORIENTED_EDGE('',*,*,#7696,.T.);
#10243=ORIENTED_EDGE('',*,*,#7889,.F.);
#10244=ORIENTED_EDGE('',*,*,#7891,.T.);
#10245=ORIENTED_EDGE('',*,*,#7892,.T.);
#10246=ORIENTED_EDGE('',*,*,#7697,.T.);
#10247=ORIENTED_EDGE('',*,*,#7890,.F.);
#10248=ORIENTED_EDGE('',*,*,#7780,.T.);
#10249=ORIENTED_EDGE('',*,*,#7893,.T.);
#10250=ORIENTED_EDGE('',*,*,#7698,.T.);
#10251=ORIENTED_EDGE('',*,*,#7892,.F.);
#10252=ORIENTED_EDGE('',*,*,#7894,.T.);
#10253=ORIENTED_EDGE('',*,*,#7895,.T.);
#10254=ORIENTED_EDGE('',*,*,#7699,.T.);
#10255=ORIENTED_EDGE('',*,*,#7893,.F.);
#10256=ORIENTED_EDGE('',*,*,#7794,.T.);
#10257=ORIENTED_EDGE('',*,*,#7896,.T.);
#10258=ORIENTED_EDGE('',*,*,#7700,.T.);
#10259=ORIENTED_EDGE('',*,*,#7895,.F.);
#10260=ORIENTED_EDGE('',*,*,#7897,.T.);
#10261=ORIENTED_EDGE('',*,*,#7898,.T.);
#10262=ORIENTED_EDGE('',*,*,#7701,.T.);
#10263=ORIENTED_EDGE('',*,*,#7896,.F.);
#10264=ORIENTED_EDGE('',*,*,#7730,.T.);
#10265=ORIENTED_EDGE('',*,*,#7888,.F.);
#10266=ORIENTED_EDGE('',*,*,#7702,.T.);
#10267=ORIENTED_EDGE('',*,*,#7898,.F.);
#10268=ORIENTED_EDGE('',*,*,#7899,.T.);
#10269=ORIENTED_EDGE('',*,*,#7873,.F.);
#10270=ORIENTED_EDGE('',*,*,#7796,.T.);
#10271=ORIENTED_EDGE('',*,*,#7673,.T.);
#10272=ORIENTED_EDGE('',*,*,#7795,.T.);
#10273=ORIENTED_EDGE('',*,*,#7894,.F.);
#10274=ORIENTED_EDGE('',*,*,#7779,.F.);
#10275=ORIENTED_EDGE('',*,*,#7879,.F.);
#10276=ORIENTED_EDGE('',*,*,#7781,.T.);
#10277=ORIENTED_EDGE('',*,*,#7891,.F.);
#10278=ORIENTED_EDGE('',*,*,#7746,.F.);
#10279=ORIENTED_EDGE('',*,*,#7653,.T.);
#10280=ORIENTED_EDGE('',*,*,#7745,.F.);
#10281=ORIENTED_EDGE('',*,*,#7705,.T.);
#10282=ORIENTED_EDGE('',*,*,#7900,.T.);
#10283=ORIENTED_EDGE('',*,*,#7901,.T.);
#10284=ORIENTED_EDGE('',*,*,#7902,.T.);
#10285=ORIENTED_EDGE('',*,*,#7900,.F.);
#10286=ORIENTED_EDGE('',*,*,#7903,.F.);
#10287=ORIENTED_EDGE('',*,*,#7904,.T.);
#10288=ORIENTED_EDGE('',*,*,#7901,.F.);
#10289=ORIENTED_EDGE('',*,*,#7902,.F.);
#10290=ORIENTED_EDGE('',*,*,#7904,.F.);
#10291=ORIENTED_EDGE('',*,*,#7905,.F.);
#10292=ORIENTED_EDGE('',*,*,#7906,.F.);
#10293=ORIENTED_EDGE('',*,*,#7907,.F.);
#10294=ORIENTED_EDGE('',*,*,#7908,.F.);
#10295=ORIENTED_EDGE('',*,*,#7909,.F.);
#10296=ORIENTED_EDGE('',*,*,#7910,.F.);
#10297=ORIENTED_EDGE('',*,*,#7911,.F.);
#10298=ORIENTED_EDGE('',*,*,#7912,.F.);
#10299=ORIENTED_EDGE('',*,*,#7913,.T.);
#10300=ORIENTED_EDGE('',*,*,#7914,.F.);
#10301=ORIENTED_EDGE('',*,*,#7907,.T.);
#10302=ORIENTED_EDGE('',*,*,#7915,.T.);
#10303=ORIENTED_EDGE('',*,*,#7690,.F.);
#10304=ORIENTED_EDGE('',*,*,#7913,.F.);
#10305=ORIENTED_EDGE('',*,*,#7906,.T.);
#10306=ORIENTED_EDGE('',*,*,#7915,.F.);
#10307=ORIENTED_EDGE('',*,*,#7905,.T.);
#10308=ORIENTED_EDGE('',*,*,#7916,.F.);
#10309=ORIENTED_EDGE('',*,*,#7914,.T.);
#10310=ORIENTED_EDGE('',*,*,#7689,.T.);
#10311=ORIENTED_EDGE('',*,*,#7691,.T.);
#10312=ORIENTED_EDGE('',*,*,#7916,.T.);
#10313=ORIENTED_EDGE('',*,*,#7908,.T.);
#10314=ORIENTED_EDGE('',*,*,#7917,.T.);
#10315=ORIENTED_EDGE('',*,*,#7918,.F.);
#10316=ORIENTED_EDGE('',*,*,#7911,.T.);
#10317=ORIENTED_EDGE('',*,*,#7919,.T.);
#10318=ORIENTED_EDGE('',*,*,#7920,.F.);
#10319=ORIENTED_EDGE('',*,*,#7917,.F.);
#10320=ORIENTED_EDGE('',*,*,#7910,.T.);
#10321=ORIENTED_EDGE('',*,*,#7919,.F.);
#10322=ORIENTED_EDGE('',*,*,#7909,.T.);
#10323=ORIENTED_EDGE('',*,*,#7921,.F.);
#10324=ORIENTED_EDGE('',*,*,#7918,.T.);
#10325=ORIENTED_EDGE('',*,*,#7922,.T.);
#10326=ORIENTED_EDGE('',*,*,#7923,.T.);
#10327=ORIENTED_EDGE('',*,*,#7921,.T.);
#10328=ORIENTED_EDGE('',*,*,#7912,.T.);
#10329=ORIENTED_EDGE('',*,*,#7655,.F.);
#10330=ORIENTED_EDGE('',*,*,#7924,.T.);
#10331=ORIENTED_EDGE('',*,*,#7922,.F.);
#10332=ORIENTED_EDGE('',*,*,#7920,.T.);
#10333=ORIENTED_EDGE('',*,*,#7923,.F.);
#10334=ORIENTED_EDGE('',*,*,#7924,.F.);
#10335=ORIENTED_EDGE('',*,*,#7708,.F.);
#10336=ORIENTED_EDGE('',*,*,#7712,.F.);
#10337=ORIENTED_EDGE('',*,*,#7716,.F.);
#10338=ORIENTED_EDGE('',*,*,#7720,.F.);
#10339=ORIENTED_EDGE('',*,*,#7925,.F.);
#10340=ORIENTED_EDGE('',*,*,#7926,.T.);
#10341=ORIENTED_EDGE('',*,*,#7927,.T.);
#10342=ORIENTED_EDGE('',*,*,#7926,.F.);
#10343=ORIENTED_EDGE('',*,*,#7928,.T.);
#10344=ORIENTED_EDGE('',*,*,#7927,.F.);
#10345=ORIENTED_EDGE('',*,*,#7928,.F.);
#10346=ORIENTED_EDGE('',*,*,#7929,.T.);
#10347=ORIENTED_EDGE('',*,*,#7930,.T.);
#10348=ORIENTED_EDGE('',*,*,#7929,.F.);
#10349=ORIENTED_EDGE('',*,*,#7930,.F.);
#10350=ORIENTED_EDGE('',*,*,#7931,.T.);
#10351=ORIENTED_EDGE('',*,*,#7931,.F.);
#10352=ORIENTED_EDGE('',*,*,#7932,.T.);
#10353=ORIENTED_EDGE('',*,*,#7933,.T.);
#10354=ORIENTED_EDGE('',*,*,#7932,.F.);
#10355=ORIENTED_EDGE('',*,*,#7903,.T.);
#10356=ORIENTED_EDGE('',*,*,#7933,.F.);
#10357=ORIENTED_EDGE('',*,*,#7862,.F.);
#10358=ORIENTED_EDGE('',*,*,#7925,.T.);
#10359=ORIENTED_EDGE('',*,*,#7867,.F.);
#10360=ORIENTED_EDGE('',*,*,#7731,.T.);
#10361=ORIENTED_EDGE('',*,*,#7897,.F.);
#10362=ORIENTED_EDGE('',*,*,#7793,.F.);
#10363=ORIENTED_EDGE('',*,*,#7885,.F.);
#10364=ORIENTED_EDGE('',*,*,#7748,.T.);
#10365=ORIENTED_EDGE('',*,*,#7899,.F.);
#10366=ORIENTED_EDGE('',*,*,#7729,.F.);
#10367=ORIENTED_EDGE('',*,*,#7856,.F.);
#10368=ORIENTED_EDGE('',*,*,#7741,.T.);
#10369=ORIENTED_EDGE('',*,*,#7848,.F.);
#10370=ORIENTED_EDGE('',*,*,#7789,.T.);
#10371=ORIENTED_EDGE('',*,*,#7934,.T.);
#10372=ORIENTED_EDGE('',*,*,#7935,.T.);
#10373=ORIENTED_EDGE('',*,*,#7936,.T.);
#10374=ORIENTED_EDGE('',*,*,#7937,.T.);
#10375=ORIENTED_EDGE('',*,*,#7935,.F.);
#10376=ORIENTED_EDGE('',*,*,#7938,.F.);
#10377=ORIENTED_EDGE('',*,*,#7934,.F.);
#10378=ORIENTED_EDGE('',*,*,#7936,.F.);
#10379=ORIENTED_EDGE('',*,*,#7937,.F.);
#10380=ORIENTED_EDGE('',*,*,#7939,.T.);
#10381=ORIENTED_EDGE('',*,*,#7940,.T.);
#10382=ORIENTED_EDGE('',*,*,#7939,.F.);
#10383=ORIENTED_EDGE('',*,*,#7941,.T.);
#10384=ORIENTED_EDGE('',*,*,#7942,.T.);
#10385=ORIENTED_EDGE('',*,*,#7943,.T.);
#10386=ORIENTED_EDGE('',*,*,#7942,.F.);
#10387=ORIENTED_EDGE('',*,*,#7944,.F.);
#10388=ORIENTED_EDGE('',*,*,#7945,.F.);
#10389=ORIENTED_EDGE('',*,*,#7946,.F.);
#10390=ORIENTED_EDGE('',*,*,#7947,.F.);
#10391=ORIENTED_EDGE('',*,*,#7948,.F.);
#10392=ORIENTED_EDGE('',*,*,#7949,.F.);
#10393=ORIENTED_EDGE('',*,*,#7950,.F.);
#10394=ORIENTED_EDGE('',*,*,#7951,.F.);
#10395=ORIENTED_EDGE('',*,*,#7941,.F.);
#10396=ORIENTED_EDGE('',*,*,#7943,.F.);
#10397=ORIENTED_EDGE('',*,*,#7952,.T.);
#10398=ORIENTED_EDGE('',*,*,#7953,.F.);
#10399=ORIENTED_EDGE('',*,*,#7954,.T.);
#10400=ORIENTED_EDGE('',*,*,#7955,.F.);
#10401=ORIENTED_EDGE('',*,*,#7956,.F.);
#10402=ORIENTED_EDGE('',*,*,#7952,.F.);
#10403=ORIENTED_EDGE('',*,*,#7957,.T.);
#10404=ORIENTED_EDGE('',*,*,#7958,.T.);
#10405=ORIENTED_EDGE('',*,*,#7959,.T.);
#10406=ORIENTED_EDGE('',*,*,#7960,.T.);
#10407=ORIENTED_EDGE('',*,*,#7944,.T.);
#10408=ORIENTED_EDGE('',*,*,#7961,.T.);
#10409=ORIENTED_EDGE('',*,*,#7962,.T.);
#10410=ORIENTED_EDGE('',*,*,#7963,.T.);
#10411=ORIENTED_EDGE('',*,*,#7964,.T.);
#10412=ORIENTED_EDGE('',*,*,#7963,.F.);
#10413=ORIENTED_EDGE('',*,*,#7965,.T.);
#10414=ORIENTED_EDGE('',*,*,#7960,.F.);
#10415=ORIENTED_EDGE('',*,*,#7966,.T.);
#10416=ORIENTED_EDGE('',*,*,#7967,.T.);
#10417=ORIENTED_EDGE('',*,*,#7968,.T.);
#10418=ORIENTED_EDGE('',*,*,#7969,.T.);
#10419=ORIENTED_EDGE('',*,*,#7970,.T.);
#10420=ORIENTED_EDGE('',*,*,#7967,.F.);
#10421=ORIENTED_EDGE('',*,*,#7971,.T.);
#10422=ORIENTED_EDGE('',*,*,#7961,.F.);
#10423=ORIENTED_EDGE('',*,*,#7972,.T.);
#10424=ORIENTED_EDGE('',*,*,#7973,.T.);
#10425=ORIENTED_EDGE('',*,*,#7974,.T.);
#10426=ORIENTED_EDGE('',*,*,#7975,.T.);
#10427=ORIENTED_EDGE('',*,*,#7976,.T.);
#10428=ORIENTED_EDGE('',*,*,#7975,.F.);
#10429=ORIENTED_EDGE('',*,*,#7977,.T.);
#10430=ORIENTED_EDGE('',*,*,#7969,.F.);
#10431=ORIENTED_EDGE('',*,*,#7978,.T.);
#10432=ORIENTED_EDGE('',*,*,#7957,.F.);
#10433=ORIENTED_EDGE('',*,*,#7979,.T.);
#10434=ORIENTED_EDGE('',*,*,#7973,.F.);
#10435=ORIENTED_EDGE('',*,*,#7980,.T.);
#10436=ORIENTED_EDGE('',*,*,#7970,.F.);
#10437=ORIENTED_EDGE('',*,*,#7981,.F.);
#10438=ORIENTED_EDGE('',*,*,#7982,.F.);
#10439=ORIENTED_EDGE('',*,*,#7977,.F.);
#10440=ORIENTED_EDGE('',*,*,#7974,.F.);
#10441=ORIENTED_EDGE('',*,*,#7979,.F.);
#10442=ORIENTED_EDGE('',*,*,#7951,.T.);
#10443=ORIENTED_EDGE('',*,*,#7983,.F.);
#10444=ORIENTED_EDGE('',*,*,#7984,.F.);
#10445=ORIENTED_EDGE('',*,*,#7985,.F.);
#10446=ORIENTED_EDGE('',*,*,#7986,.T.);
#10447=ORIENTED_EDGE('',*,*,#7987,.F.);
#10448=ORIENTED_EDGE('',*,*,#7988,.T.);
#10449=ORIENTED_EDGE('',*,*,#7989,.F.);
#10450=ORIENTED_EDGE('',*,*,#7981,.T.);
#10451=ORIENTED_EDGE('',*,*,#7976,.F.);
#10452=ORIENTED_EDGE('',*,*,#7978,.F.);
#10453=ORIENTED_EDGE('',*,*,#7968,.F.);
#10454=ORIENTED_EDGE('',*,*,#7972,.F.);
#10455=ORIENTED_EDGE('',*,*,#7964,.F.);
#10456=ORIENTED_EDGE('',*,*,#7966,.F.);
#10457=ORIENTED_EDGE('',*,*,#7959,.F.);
#10458=ORIENTED_EDGE('',*,*,#7990,.T.);
#10459=ORIENTED_EDGE('',*,*,#7991,.T.);
#10460=ORIENTED_EDGE('',*,*,#7990,.F.);
#10461=ORIENTED_EDGE('',*,*,#7958,.F.);
#10462=ORIENTED_EDGE('',*,*,#7980,.F.);
#10463=ORIENTED_EDGE('',*,*,#7992,.T.);
#10464=ORIENTED_EDGE('',*,*,#7993,.T.);
#10465=ORIENTED_EDGE('',*,*,#7994,.T.);
#10466=ORIENTED_EDGE('',*,*,#7946,.T.);
#10467=ORIENTED_EDGE('',*,*,#7995,.T.);
#10468=ORIENTED_EDGE('',*,*,#7996,.T.);
#10469=ORIENTED_EDGE('',*,*,#7997,.T.);
#10470=ORIENTED_EDGE('',*,*,#7998,.T.);
#10471=ORIENTED_EDGE('',*,*,#7999,.T.);
#10472=ORIENTED_EDGE('',*,*,#7997,.F.);
#10473=ORIENTED_EDGE('',*,*,#8000,.T.);
#10474=ORIENTED_EDGE('',*,*,#7994,.F.);
#10475=ORIENTED_EDGE('',*,*,#8001,.T.);
#10476=ORIENTED_EDGE('',*,*,#8002,.T.);
#10477=ORIENTED_EDGE('',*,*,#8003,.T.);
#10478=ORIENTED_EDGE('',*,*,#8004,.T.);
#10479=ORIENTED_EDGE('',*,*,#8005,.T.);
#10480=ORIENTED_EDGE('',*,*,#8002,.F.);
#10481=ORIENTED_EDGE('',*,*,#8006,.T.);
#10482=ORIENTED_EDGE('',*,*,#7995,.F.);
#10483=ORIENTED_EDGE('',*,*,#8007,.T.);
#10484=ORIENTED_EDGE('',*,*,#8008,.T.);
#10485=ORIENTED_EDGE('',*,*,#8009,.T.);
#10486=ORIENTED_EDGE('',*,*,#8010,.T.);
#10487=ORIENTED_EDGE('',*,*,#8011,.T.);
#10488=ORIENTED_EDGE('',*,*,#8010,.F.);
#10489=ORIENTED_EDGE('',*,*,#8012,.T.);
#10490=ORIENTED_EDGE('',*,*,#8004,.F.);
#10491=ORIENTED_EDGE('',*,*,#8013,.T.);
#10492=ORIENTED_EDGE('',*,*,#7992,.F.);
#10493=ORIENTED_EDGE('',*,*,#8014,.T.);
#10494=ORIENTED_EDGE('',*,*,#8008,.F.);
#10495=ORIENTED_EDGE('',*,*,#8015,.T.);
#10496=ORIENTED_EDGE('',*,*,#8005,.F.);
#10497=ORIENTED_EDGE('',*,*,#8016,.F.);
#10498=ORIENTED_EDGE('',*,*,#8017,.F.);
#10499=ORIENTED_EDGE('',*,*,#7971,.F.);
#10500=ORIENTED_EDGE('',*,*,#7982,.T.);
#10501=ORIENTED_EDGE('',*,*,#8018,.T.);
#10502=ORIENTED_EDGE('',*,*,#8019,.T.);
#10503=ORIENTED_EDGE('',*,*,#8020,.T.);
#10504=ORIENTED_EDGE('',*,*,#8016,.T.);
#10505=ORIENTED_EDGE('',*,*,#8012,.F.);
#10506=ORIENTED_EDGE('',*,*,#8009,.F.);
#10507=ORIENTED_EDGE('',*,*,#8014,.F.);
#10508=ORIENTED_EDGE('',*,*,#7945,.T.);
#10509=ORIENTED_EDGE('',*,*,#7965,.F.);
#10510=ORIENTED_EDGE('',*,*,#7962,.F.);
#10511=ORIENTED_EDGE('',*,*,#8011,.F.);
#10512=ORIENTED_EDGE('',*,*,#8013,.F.);
#10513=ORIENTED_EDGE('',*,*,#8003,.F.);
#10514=ORIENTED_EDGE('',*,*,#8007,.F.);
#10515=ORIENTED_EDGE('',*,*,#7999,.F.);
#10516=ORIENTED_EDGE('',*,*,#8021,.T.);
#10517=ORIENTED_EDGE('',*,*,#8022,.T.);
#10518=ORIENTED_EDGE('',*,*,#8021,.F.);
#10519=ORIENTED_EDGE('',*,*,#7998,.F.);
#10520=ORIENTED_EDGE('',*,*,#8001,.F.);
#10521=ORIENTED_EDGE('',*,*,#7993,.F.);
#10522=ORIENTED_EDGE('',*,*,#8015,.F.);
#10523=ORIENTED_EDGE('',*,*,#8023,.T.);
#10524=ORIENTED_EDGE('',*,*,#8024,.T.);
#10525=ORIENTED_EDGE('',*,*,#8025,.T.);
#10526=ORIENTED_EDGE('',*,*,#8026,.T.);
#10527=ORIENTED_EDGE('',*,*,#8027,.T.);
#10528=ORIENTED_EDGE('',*,*,#8028,.T.);
#10529=ORIENTED_EDGE('',*,*,#8029,.T.);
#10530=ORIENTED_EDGE('',*,*,#8030,.T.);
#10531=ORIENTED_EDGE('',*,*,#8029,.F.);
#10532=ORIENTED_EDGE('',*,*,#8031,.T.);
#10533=ORIENTED_EDGE('',*,*,#8025,.F.);
#10534=ORIENTED_EDGE('',*,*,#8032,.T.);
#10535=ORIENTED_EDGE('',*,*,#8033,.T.);
#10536=ORIENTED_EDGE('',*,*,#8034,.T.);
#10537=ORIENTED_EDGE('',*,*,#8035,.T.);
#10538=ORIENTED_EDGE('',*,*,#8036,.T.);
#10539=ORIENTED_EDGE('',*,*,#7950,.T.);
#10540=ORIENTED_EDGE('',*,*,#8033,.F.);
#10541=ORIENTED_EDGE('',*,*,#8037,.T.);
#10542=ORIENTED_EDGE('',*,*,#8027,.F.);
#10543=ORIENTED_EDGE('',*,*,#8038,.T.);
#10544=ORIENTED_EDGE('',*,*,#8039,.T.);
#10545=ORIENTED_EDGE('',*,*,#7984,.T.);
#10546=ORIENTED_EDGE('',*,*,#8040,.T.);
#10547=ORIENTED_EDGE('',*,*,#8041,.T.);
#10548=ORIENTED_EDGE('',*,*,#8040,.F.);
#10549=ORIENTED_EDGE('',*,*,#7983,.T.);
#10550=ORIENTED_EDGE('',*,*,#8036,.F.);
#10551=ORIENTED_EDGE('',*,*,#8042,.T.);
#10552=ORIENTED_EDGE('',*,*,#8023,.F.);
#10553=ORIENTED_EDGE('',*,*,#7985,.T.);
#10554=ORIENTED_EDGE('',*,*,#8039,.F.);
#10555=ORIENTED_EDGE('',*,*,#8043,.T.);
#10556=ORIENTED_EDGE('',*,*,#8041,.F.);
#10557=ORIENTED_EDGE('',*,*,#8042,.F.);
#10558=ORIENTED_EDGE('',*,*,#8035,.F.);
#10559=ORIENTED_EDGE('',*,*,#8044,.T.);
#10560=ORIENTED_EDGE('',*,*,#8045,.T.);
#10561=ORIENTED_EDGE('',*,*,#8044,.F.);
#10562=ORIENTED_EDGE('',*,*,#8034,.F.);
#10563=ORIENTED_EDGE('',*,*,#8038,.F.);
#10564=ORIENTED_EDGE('',*,*,#8030,.F.);
#10565=ORIENTED_EDGE('',*,*,#8032,.F.);
#10566=ORIENTED_EDGE('',*,*,#8024,.F.);
#10567=ORIENTED_EDGE('',*,*,#8043,.F.);
#10568=ORIENTED_EDGE('',*,*,#8046,.T.);
#10569=ORIENTED_EDGE('',*,*,#8047,.T.);
#10570=ORIENTED_EDGE('',*,*,#8048,.T.);
#10571=ORIENTED_EDGE('',*,*,#7948,.T.);
#10572=ORIENTED_EDGE('',*,*,#8049,.T.);
#10573=ORIENTED_EDGE('',*,*,#8050,.T.);
#10574=ORIENTED_EDGE('',*,*,#8051,.T.);
#10575=ORIENTED_EDGE('',*,*,#8052,.T.);
#10576=ORIENTED_EDGE('',*,*,#8051,.F.);
#10577=ORIENTED_EDGE('',*,*,#8053,.T.);
#10578=ORIENTED_EDGE('',*,*,#8048,.F.);
#10579=ORIENTED_EDGE('',*,*,#8054,.T.);
#10580=ORIENTED_EDGE('',*,*,#8055,.T.);
#10581=ORIENTED_EDGE('',*,*,#8056,.T.);
#10582=ORIENTED_EDGE('',*,*,#8057,.T.);
#10583=ORIENTED_EDGE('',*,*,#8058,.T.);
#10584=ORIENTED_EDGE('',*,*,#8055,.F.);
#10585=ORIENTED_EDGE('',*,*,#8059,.T.);
#10586=ORIENTED_EDGE('',*,*,#8049,.F.);
#10587=ORIENTED_EDGE('',*,*,#8060,.T.);
#10588=ORIENTED_EDGE('',*,*,#8061,.T.);
#10589=ORIENTED_EDGE('',*,*,#8062,.T.);
#10590=ORIENTED_EDGE('',*,*,#8063,.T.);
#10591=ORIENTED_EDGE('',*,*,#8064,.T.);
#10592=ORIENTED_EDGE('',*,*,#8065,.T.);
#10593=ORIENTED_EDGE('',*,*,#8063,.F.);
#10594=ORIENTED_EDGE('',*,*,#8066,.T.);
#10595=ORIENTED_EDGE('',*,*,#8057,.F.);
#10596=ORIENTED_EDGE('',*,*,#8067,.T.);
#10597=ORIENTED_EDGE('',*,*,#8046,.F.);
#10598=ORIENTED_EDGE('',*,*,#8068,.T.);
#10599=ORIENTED_EDGE('',*,*,#8061,.F.);
#10600=ORIENTED_EDGE('',*,*,#8069,.T.);
#10601=ORIENTED_EDGE('',*,*,#8058,.F.);
#10602=ORIENTED_EDGE('',*,*,#8070,.F.);
#10603=ORIENTED_EDGE('',*,*,#8071,.F.);
#10604=ORIENTED_EDGE('',*,*,#8006,.F.);
#10605=ORIENTED_EDGE('',*,*,#8017,.T.);
#10606=ORIENTED_EDGE('',*,*,#8072,.T.);
#10607=ORIENTED_EDGE('',*,*,#8073,.T.);
#10608=ORIENTED_EDGE('',*,*,#8074,.T.);
#10609=ORIENTED_EDGE('',*,*,#8070,.T.);
#10610=ORIENTED_EDGE('',*,*,#8066,.F.);
#10611=ORIENTED_EDGE('',*,*,#8062,.F.);
#10612=ORIENTED_EDGE('',*,*,#8068,.F.);
#10613=ORIENTED_EDGE('',*,*,#7947,.T.);
#10614=ORIENTED_EDGE('',*,*,#8000,.F.);
#10615=ORIENTED_EDGE('',*,*,#7996,.F.);
#10616=ORIENTED_EDGE('',*,*,#8064,.F.);
#10617=ORIENTED_EDGE('',*,*,#8067,.F.);
#10618=ORIENTED_EDGE('',*,*,#8056,.F.);
#10619=ORIENTED_EDGE('',*,*,#8060,.F.);
#10620=ORIENTED_EDGE('',*,*,#8052,.F.);
#10621=ORIENTED_EDGE('',*,*,#8054,.F.);
#10622=ORIENTED_EDGE('',*,*,#8047,.F.);
#10623=ORIENTED_EDGE('',*,*,#8069,.F.);
#10624=ORIENTED_EDGE('',*,*,#8065,.F.);
#10625=ORIENTED_EDGE('',*,*,#8075,.T.);
#10626=ORIENTED_EDGE('',*,*,#8076,.T.);
#10627=ORIENTED_EDGE('',*,*,#8075,.F.);
#10628=ORIENTED_EDGE('',*,*,#8077,.F.);
#10629=ORIENTED_EDGE('',*,*,#8078,.T.);
#10630=ORIENTED_EDGE('',*,*,#8079,.T.);
#10631=ORIENTED_EDGE('',*,*,#8080,.T.);
#10632=ORIENTED_EDGE('',*,*,#8079,.F.);
#10633=ORIENTED_EDGE('',*,*,#8081,.T.);
#10634=ORIENTED_EDGE('',*,*,#8082,.T.);
#10635=ORIENTED_EDGE('',*,*,#8083,.T.);
#10636=ORIENTED_EDGE('',*,*,#8077,.T.);
#10637=ORIENTED_EDGE('',*,*,#8084,.T.);
#10638=ORIENTED_EDGE('',*,*,#8085,.T.);
#10639=ORIENTED_EDGE('',*,*,#8086,.T.);
#10640=ORIENTED_EDGE('',*,*,#8087,.T.);
#10641=ORIENTED_EDGE('',*,*,#8088,.T.);
#10642=ORIENTED_EDGE('',*,*,#8089,.T.);
#10643=ORIENTED_EDGE('',*,*,#8090,.T.);
#10644=ORIENTED_EDGE('',*,*,#8091,.T.);
#10645=ORIENTED_EDGE('',*,*,#8090,.F.);
#10646=ORIENTED_EDGE('',*,*,#8092,.T.);
#10647=ORIENTED_EDGE('',*,*,#8082,.F.);
#10648=ORIENTED_EDGE('',*,*,#8093,.T.);
#10649=ORIENTED_EDGE('',*,*,#8085,.F.);
#10650=ORIENTED_EDGE('',*,*,#8094,.T.);
#10651=ORIENTED_EDGE('',*,*,#8095,.T.);
#10652=ORIENTED_EDGE('',*,*,#8086,.F.);
#10653=ORIENTED_EDGE('',*,*,#8094,.F.);
#10654=ORIENTED_EDGE('',*,*,#8084,.F.);
#10655=ORIENTED_EDGE('',*,*,#8080,.F.);
#10656=ORIENTED_EDGE('',*,*,#8083,.F.);
#10657=ORIENTED_EDGE('',*,*,#8092,.F.);
#10658=ORIENTED_EDGE('',*,*,#8089,.F.);
#10659=ORIENTED_EDGE('',*,*,#8096,.F.);
#10660=ORIENTED_EDGE('',*,*,#8097,.T.);
#10661=ORIENTED_EDGE('',*,*,#8098,.T.);
#10662=ORIENTED_EDGE('',*,*,#8099,.T.);
#10663=ORIENTED_EDGE('',*,*,#8100,.T.);
#10664=ORIENTED_EDGE('',*,*,#8101,.F.);
#10665=ORIENTED_EDGE('',*,*,#8102,.T.);
#10666=ORIENTED_EDGE('',*,*,#8103,.T.);
#10667=ORIENTED_EDGE('',*,*,#8104,.T.);
#10668=ORIENTED_EDGE('',*,*,#8105,.T.);
#10669=ORIENTED_EDGE('',*,*,#8101,.T.);
#10670=ORIENTED_EDGE('',*,*,#8106,.T.);
#10671=ORIENTED_EDGE('',*,*,#8107,.F.);
#10672=ORIENTED_EDGE('',*,*,#8108,.T.);
#10673=ORIENTED_EDGE('',*,*,#8107,.T.);
#10674=ORIENTED_EDGE('',*,*,#8109,.T.);
#10675=ORIENTED_EDGE('',*,*,#8110,.T.);
#10676=ORIENTED_EDGE('',*,*,#8111,.T.);
#10677=ORIENTED_EDGE('',*,*,#8112,.T.);
#10678=ORIENTED_EDGE('',*,*,#8113,.T.);
#10679=ORIENTED_EDGE('',*,*,#8114,.T.);
#10680=ORIENTED_EDGE('',*,*,#8115,.T.);
#10681=ORIENTED_EDGE('',*,*,#8112,.F.);
#10682=ORIENTED_EDGE('',*,*,#8116,.T.);
#10683=ORIENTED_EDGE('',*,*,#8110,.F.);
#10684=ORIENTED_EDGE('',*,*,#8117,.T.);
#10685=ORIENTED_EDGE('',*,*,#8103,.F.);
#10686=ORIENTED_EDGE('',*,*,#8118,.T.);
#10687=ORIENTED_EDGE('',*,*,#8119,.T.);
#10688=ORIENTED_EDGE('',*,*,#8104,.F.);
#10689=ORIENTED_EDGE('',*,*,#8118,.F.);
#10690=ORIENTED_EDGE('',*,*,#8102,.F.);
#10691=ORIENTED_EDGE('',*,*,#8108,.F.);
#10692=ORIENTED_EDGE('',*,*,#8111,.F.);
#10693=ORIENTED_EDGE('',*,*,#8116,.F.);
#10694=ORIENTED_EDGE('',*,*,#8120,.T.);
#10695=ORIENTED_EDGE('',*,*,#8121,.T.);
#10696=ORIENTED_EDGE('',*,*,#8122,.T.);
#10697=ORIENTED_EDGE('',*,*,#8091,.F.);
#10698=ORIENTED_EDGE('',*,*,#8123,.F.);
#10699=ORIENTED_EDGE('',*,*,#8124,.F.);
#10700=ORIENTED_EDGE('',*,*,#8125,.F.);
#10701=ORIENTED_EDGE('',*,*,#8126,.F.);
#10702=ORIENTED_EDGE('',*,*,#8127,.F.);
#10703=ORIENTED_EDGE('',*,*,#8128,.F.);
#10704=ORIENTED_EDGE('',*,*,#8129,.F.);
#10705=ORIENTED_EDGE('',*,*,#8130,.F.);
#10706=ORIENTED_EDGE('',*,*,#8131,.F.);
#10707=ORIENTED_EDGE('',*,*,#8132,.F.);
#10708=ORIENTED_EDGE('',*,*,#8133,.F.);
#10709=ORIENTED_EDGE('',*,*,#8134,.F.);
#10710=ORIENTED_EDGE('',*,*,#8135,.F.);
#10711=ORIENTED_EDGE('',*,*,#8136,.F.);
#10712=ORIENTED_EDGE('',*,*,#8120,.F.);
#10713=ORIENTED_EDGE('',*,*,#8115,.F.);
#10714=ORIENTED_EDGE('',*,*,#8137,.F.);
#10715=ORIENTED_EDGE('',*,*,#7988,.F.);
#10716=ORIENTED_EDGE('',*,*,#8138,.T.);
#10717=ORIENTED_EDGE('',*,*,#8139,.T.);
#10718=ORIENTED_EDGE('',*,*,#8140,.T.);
#10719=ORIENTED_EDGE('',*,*,#8141,.T.);
#10720=ORIENTED_EDGE('',*,*,#8140,.F.);
#10721=ORIENTED_EDGE('',*,*,#8142,.F.);
#10722=ORIENTED_EDGE('',*,*,#8143,.F.);
#10723=ORIENTED_EDGE('',*,*,#8144,.F.);
#10724=ORIENTED_EDGE('',*,*,#8145,.F.);
#10725=ORIENTED_EDGE('',*,*,#8146,.F.);
#10726=ORIENTED_EDGE('',*,*,#8147,.F.);
#10727=ORIENTED_EDGE('',*,*,#8148,.F.);
#10728=ORIENTED_EDGE('',*,*,#8149,.F.);
#10729=ORIENTED_EDGE('',*,*,#8139,.F.);
#10730=ORIENTED_EDGE('',*,*,#8141,.F.);
#10731=ORIENTED_EDGE('',*,*,#8150,.T.);
#10732=ORIENTED_EDGE('',*,*,#8151,.T.);
#10733=ORIENTED_EDGE('',*,*,#8150,.F.);
#10734=ORIENTED_EDGE('',*,*,#8146,.T.);
#10735=ORIENTED_EDGE('',*,*,#8152,.T.);
#10736=ORIENTED_EDGE('',*,*,#8153,.T.);
#10737=ORIENTED_EDGE('',*,*,#8152,.F.);
#10738=ORIENTED_EDGE('',*,*,#8153,.F.);
#10739=ORIENTED_EDGE('',*,*,#8154,.T.);
#10740=ORIENTED_EDGE('',*,*,#8155,.T.);
#10741=ORIENTED_EDGE('',*,*,#8154,.F.);
#10742=ORIENTED_EDGE('',*,*,#8149,.T.);
#10743=ORIENTED_EDGE('',*,*,#8156,.T.);
#10744=ORIENTED_EDGE('',*,*,#8157,.T.);
#10745=ORIENTED_EDGE('',*,*,#8156,.F.);
#10746=ORIENTED_EDGE('',*,*,#8157,.F.);
#10747=ORIENTED_EDGE('',*,*,#8158,.T.);
#10748=ORIENTED_EDGE('',*,*,#8159,.T.);
#10749=ORIENTED_EDGE('',*,*,#8158,.F.);
#10750=ORIENTED_EDGE('',*,*,#8147,.T.);
#10751=ORIENTED_EDGE('',*,*,#8160,.T.);
#10752=ORIENTED_EDGE('',*,*,#8161,.T.);
#10753=ORIENTED_EDGE('',*,*,#8160,.F.);
#10754=ORIENTED_EDGE('',*,*,#8161,.F.);
#10755=ORIENTED_EDGE('',*,*,#8162,.T.);
#10756=ORIENTED_EDGE('',*,*,#8163,.T.);
#10757=ORIENTED_EDGE('',*,*,#8162,.F.);
#10758=ORIENTED_EDGE('',*,*,#8148,.T.);
#10759=ORIENTED_EDGE('',*,*,#8164,.T.);
#10760=ORIENTED_EDGE('',*,*,#8165,.T.);
#10761=ORIENTED_EDGE('',*,*,#8164,.F.);
#10762=ORIENTED_EDGE('',*,*,#8165,.F.);
#10763=ORIENTED_EDGE('',*,*,#8166,.T.);
#10764=ORIENTED_EDGE('',*,*,#8167,.F.);
#10765=ORIENTED_EDGE('',*,*,#8168,.T.);
#10766=ORIENTED_EDGE('',*,*,#8169,.F.);
#10767=ORIENTED_EDGE('',*,*,#8170,.F.);
#10768=ORIENTED_EDGE('',*,*,#8166,.F.);
#10769=ORIENTED_EDGE('',*,*,#8171,.T.);
#10770=ORIENTED_EDGE('',*,*,#8172,.T.);
#10771=ORIENTED_EDGE('',*,*,#8171,.F.);
#10772=ORIENTED_EDGE('',*,*,#8169,.T.);
#10773=ORIENTED_EDGE('',*,*,#8167,.T.);
#10774=ORIENTED_EDGE('',*,*,#8170,.T.);
#10775=ORIENTED_EDGE('',*,*,#8173,.F.);
#10776=ORIENTED_EDGE('',*,*,#8174,.T.);
#10777=ORIENTED_EDGE('',*,*,#8172,.F.);
#10778=ORIENTED_EDGE('',*,*,#8174,.F.);
#10779=ORIENTED_EDGE('',*,*,#8175,.T.);
#10780=ORIENTED_EDGE('',*,*,#8176,.T.);
#10781=ORIENTED_EDGE('',*,*,#8177,.T.);
#10782=ORIENTED_EDGE('',*,*,#8178,.T.);
#10783=ORIENTED_EDGE('',*,*,#8179,.F.);
#10784=ORIENTED_EDGE('',*,*,#8180,.F.);
#10785=ORIENTED_EDGE('',*,*,#8181,.F.);
#10786=ORIENTED_EDGE('',*,*,#8182,.T.);
#10787=ORIENTED_EDGE('',*,*,#8183,.T.);
#10788=ORIENTED_EDGE('',*,*,#8180,.T.);
#10789=ORIENTED_EDGE('',*,*,#8142,.T.);
#10790=ORIENTED_EDGE('',*,*,#8184,.T.);
#10791=ORIENTED_EDGE('',*,*,#8185,.T.);
#10792=ORIENTED_EDGE('',*,*,#8181,.T.);
#10793=ORIENTED_EDGE('',*,*,#8186,.T.);
#10794=ORIENTED_EDGE('',*,*,#8187,.T.);
#10795=ORIENTED_EDGE('',*,*,#8143,.T.);
#10796=ORIENTED_EDGE('',*,*,#8179,.T.);
#10797=ORIENTED_EDGE('',*,*,#8188,.T.);
#10798=ORIENTED_EDGE('',*,*,#8182,.F.);
#10799=ORIENTED_EDGE('',*,*,#8189,.T.);
#10800=ORIENTED_EDGE('',*,*,#8175,.F.);
#10801=ORIENTED_EDGE('',*,*,#8190,.T.);
#10802=ORIENTED_EDGE('',*,*,#8191,.T.);
#10803=ORIENTED_EDGE('',*,*,#8192,.T.);
#10804=ORIENTED_EDGE('',*,*,#8131,.T.);
#10805=ORIENTED_EDGE('',*,*,#8190,.F.);
#10806=ORIENTED_EDGE('',*,*,#8193,.T.);
#10807=ORIENTED_EDGE('',*,*,#8187,.F.);
#10808=ORIENTED_EDGE('',*,*,#8176,.F.);
#10809=ORIENTED_EDGE('',*,*,#8194,.F.);
#10810=ORIENTED_EDGE('',*,*,#8195,.F.);
#10811=ORIENTED_EDGE('',*,*,#8196,.F.);
#10812=ORIENTED_EDGE('',*,*,#8189,.F.);
#10813=ORIENTED_EDGE('',*,*,#8145,.T.);
#10814=ORIENTED_EDGE('',*,*,#8197,.T.);
#10815=ORIENTED_EDGE('',*,*,#8194,.T.);
#10816=ORIENTED_EDGE('',*,*,#8193,.F.);
#10817=ORIENTED_EDGE('',*,*,#8130,.T.);
#10818=ORIENTED_EDGE('',*,*,#8198,.F.);
#10819=ORIENTED_EDGE('',*,*,#8144,.T.);
#10820=ORIENTED_EDGE('',*,*,#8199,.F.);
#10821=ORIENTED_EDGE('',*,*,#8072,.F.);
#10822=ORIENTED_EDGE('',*,*,#8020,.F.);
#10823=ORIENTED_EDGE('',*,*,#8074,.F.);
#10824=ORIENTED_EDGE('',*,*,#8200,.F.);
#10825=ORIENTED_EDGE('',*,*,#8201,.F.);
#10826=ORIENTED_EDGE('',*,*,#8202,.T.);
#10827=ORIENTED_EDGE('',*,*,#8203,.T.);
#10828=ORIENTED_EDGE('',*,*,#8200,.T.);
#10829=ORIENTED_EDGE('',*,*,#8204,.T.);
#10830=ORIENTED_EDGE('',*,*,#8037,.F.);
#10831=ORIENTED_EDGE('',*,*,#7949,.T.);
#10832=ORIENTED_EDGE('',*,*,#8053,.F.);
#10833=ORIENTED_EDGE('',*,*,#8050,.F.);
#10834=ORIENTED_EDGE('',*,*,#8059,.F.);
#10835=ORIENTED_EDGE('',*,*,#8071,.T.);
#10836=ORIENTED_EDGE('',*,*,#8201,.T.);
#10837=ORIENTED_EDGE('',*,*,#8205,.T.);
#10838=ORIENTED_EDGE('',*,*,#8206,.T.);
#10839=ORIENTED_EDGE('',*,*,#8207,.T.);
#10840=ORIENTED_EDGE('',*,*,#8031,.F.);
#10841=ORIENTED_EDGE('',*,*,#8028,.F.);
#10842=ORIENTED_EDGE('',*,*,#8206,.F.);
#10843=ORIENTED_EDGE('',*,*,#8208,.T.);
#10844=ORIENTED_EDGE('',*,*,#7987,.T.);
#10845=ORIENTED_EDGE('',*,*,#8018,.F.);
#10846=ORIENTED_EDGE('',*,*,#7989,.T.);
#10847=ORIENTED_EDGE('',*,*,#8209,.T.);
#10848=ORIENTED_EDGE('',*,*,#8210,.T.);
#10849=ORIENTED_EDGE('',*,*,#8211,.T.);
#10850=ORIENTED_EDGE('',*,*,#8199,.T.);
#10851=ORIENTED_EDGE('',*,*,#8212,.T.);
#10852=ORIENTED_EDGE('',*,*,#8208,.F.);
#10853=ORIENTED_EDGE('',*,*,#8213,.T.);
#10854=ORIENTED_EDGE('',*,*,#8096,.T.);
#10855=ORIENTED_EDGE('',*,*,#8088,.F.);
#10856=ORIENTED_EDGE('',*,*,#8138,.F.);
#10857=ORIENTED_EDGE('',*,*,#8205,.F.);
#10858=ORIENTED_EDGE('',*,*,#8203,.F.);
#10859=ORIENTED_EDGE('',*,*,#8214,.F.);
#10860=ORIENTED_EDGE('',*,*,#8097,.F.);
#10861=ORIENTED_EDGE('',*,*,#8213,.F.);
#10862=ORIENTED_EDGE('',*,*,#8026,.F.);
#10863=ORIENTED_EDGE('',*,*,#8207,.F.);
#10864=ORIENTED_EDGE('',*,*,#7986,.F.);
#10865=ORIENTED_EDGE('',*,*,#8215,.F.);
#10866=ORIENTED_EDGE('',*,*,#8216,.F.);
#10867=ORIENTED_EDGE('',*,*,#8217,.F.);
#10868=ORIENTED_EDGE('',*,*,#8204,.F.);
#10869=ORIENTED_EDGE('',*,*,#8073,.F.);
#10870=ORIENTED_EDGE('',*,*,#8211,.F.);
#10871=ORIENTED_EDGE('',*,*,#8218,.F.);
#10872=ORIENTED_EDGE('',*,*,#8219,.F.);
#10873=ORIENTED_EDGE('',*,*,#8220,.F.);
#10874=ORIENTED_EDGE('',*,*,#8186,.F.);
#10875=ORIENTED_EDGE('',*,*,#8183,.F.);
#10876=ORIENTED_EDGE('',*,*,#8178,.F.);
#10877=ORIENTED_EDGE('',*,*,#8221,.F.);
#10878=ORIENTED_EDGE('',*,*,#8222,.T.);
#10879=ORIENTED_EDGE('',*,*,#8223,.T.);
#10880=ORIENTED_EDGE('',*,*,#8224,.T.);
#10881=ORIENTED_EDGE('',*,*,#8225,.T.);
#10882=ORIENTED_EDGE('',*,*,#8221,.T.);
#10883=ORIENTED_EDGE('',*,*,#8226,.T.);
#10884=ORIENTED_EDGE('',*,*,#8227,.T.);
#10885=ORIENTED_EDGE('',*,*,#8228,.T.);
#10886=ORIENTED_EDGE('',*,*,#8226,.F.);
#10887=ORIENTED_EDGE('',*,*,#8228,.F.);
#10888=ORIENTED_EDGE('',*,*,#8229,.T.);
#10889=ORIENTED_EDGE('',*,*,#8230,.T.);
#10890=ORIENTED_EDGE('',*,*,#8229,.F.);
#10891=ORIENTED_EDGE('',*,*,#8227,.F.);
#10892=ORIENTED_EDGE('',*,*,#8231,.T.);
#10893=ORIENTED_EDGE('',*,*,#8232,.T.);
#10894=ORIENTED_EDGE('',*,*,#8202,.F.);
#10895=ORIENTED_EDGE('',*,*,#8217,.T.);
#10896=ORIENTED_EDGE('',*,*,#8233,.T.);
#10897=ORIENTED_EDGE('',*,*,#8234,.T.);
#10898=ORIENTED_EDGE('',*,*,#8231,.F.);
#10899=ORIENTED_EDGE('',*,*,#8216,.T.);
#10900=ORIENTED_EDGE('',*,*,#8235,.T.);
#10901=ORIENTED_EDGE('',*,*,#8233,.F.);
#10902=ORIENTED_EDGE('',*,*,#8215,.T.);
#10903=ORIENTED_EDGE('',*,*,#8177,.F.);
#10904=ORIENTED_EDGE('',*,*,#8236,.T.);
#10905=ORIENTED_EDGE('',*,*,#8237,.T.);
#10906=ORIENTED_EDGE('',*,*,#8238,.T.);
#10907=ORIENTED_EDGE('',*,*,#7953,.T.);
#10908=ORIENTED_EDGE('',*,*,#7956,.T.);
#10909=ORIENTED_EDGE('',*,*,#8236,.F.);
#10910=ORIENTED_EDGE('',*,*,#7955,.T.);
#10911=ORIENTED_EDGE('',*,*,#8238,.F.);
#10912=ORIENTED_EDGE('',*,*,#8239,.T.);
#10913=ORIENTED_EDGE('',*,*,#8230,.F.);
#10914=ORIENTED_EDGE('',*,*,#8240,.T.);
#10915=ORIENTED_EDGE('',*,*,#8173,.T.);
#10916=ORIENTED_EDGE('',*,*,#8237,.F.);
#10917=ORIENTED_EDGE('',*,*,#8239,.F.);
#10918=ORIENTED_EDGE('',*,*,#8098,.F.);
#10919=ORIENTED_EDGE('',*,*,#8241,.T.);
#10920=ORIENTED_EDGE('',*,*,#8242,.T.);
#10921=ORIENTED_EDGE('',*,*,#8243,.T.);
#10922=ORIENTED_EDGE('',*,*,#8243,.F.);
#10923=ORIENTED_EDGE('',*,*,#8244,.F.);
#10924=ORIENTED_EDGE('',*,*,#8245,.F.);
#10925=ORIENTED_EDGE('',*,*,#8099,.F.);
#10926=ORIENTED_EDGE('',*,*,#8246,.T.);
#10927=ORIENTED_EDGE('',*,*,#8247,.T.);
#10928=ORIENTED_EDGE('',*,*,#8248,.T.);
#10929=ORIENTED_EDGE('',*,*,#8249,.T.);
#10930=ORIENTED_EDGE('',*,*,#8250,.T.);
#10931=ORIENTED_EDGE('',*,*,#8250,.F.);
#10932=ORIENTED_EDGE('',*,*,#8251,.F.);
#10933=ORIENTED_EDGE('',*,*,#8252,.F.);
#10934=ORIENTED_EDGE('',*,*,#8253,.F.);
#10935=ORIENTED_EDGE('',*,*,#8254,.F.);
#10936=ORIENTED_EDGE('',*,*,#8255,.T.);
#10937=ORIENTED_EDGE('',*,*,#8256,.T.);
#10938=ORIENTED_EDGE('',*,*,#8257,.T.);
#10939=ORIENTED_EDGE('',*,*,#8258,.T.);
#10940=ORIENTED_EDGE('',*,*,#8259,.T.);
#10941=ORIENTED_EDGE('',*,*,#8257,.F.);
#10942=ORIENTED_EDGE('',*,*,#8260,.F.);
#10943=ORIENTED_EDGE('',*,*,#8261,.F.);
#10944=ORIENTED_EDGE('',*,*,#8262,.F.);
#10945=ORIENTED_EDGE('',*,*,#8263,.T.);
#10946=ORIENTED_EDGE('',*,*,#8264,.T.);
#10947=ORIENTED_EDGE('',*,*,#8265,.T.);
#10948=ORIENTED_EDGE('',*,*,#8266,.T.);
#10949=ORIENTED_EDGE('',*,*,#8267,.T.);
#10950=ORIENTED_EDGE('',*,*,#8265,.F.);
#10951=ORIENTED_EDGE('',*,*,#8268,.F.);
#10952=ORIENTED_EDGE('',*,*,#8269,.F.);
#10953=ORIENTED_EDGE('',*,*,#8270,.F.);
#10954=ORIENTED_EDGE('',*,*,#8271,.T.);
#10955=ORIENTED_EDGE('',*,*,#8272,.T.);
#10956=ORIENTED_EDGE('',*,*,#8219,.T.);
#10957=ORIENTED_EDGE('',*,*,#8273,.T.);
#10958=ORIENTED_EDGE('',*,*,#8274,.T.);
#10959=ORIENTED_EDGE('',*,*,#8254,.T.);
#10960=ORIENTED_EDGE('',*,*,#8273,.F.);
#10961=ORIENTED_EDGE('',*,*,#8218,.T.);
#10962=ORIENTED_EDGE('',*,*,#8210,.F.);
#10963=ORIENTED_EDGE('',*,*,#8220,.T.);
#10964=ORIENTED_EDGE('',*,*,#8272,.F.);
#10965=ORIENTED_EDGE('',*,*,#8275,.T.);
#10966=ORIENTED_EDGE('',*,*,#8184,.F.);
#10967=ORIENTED_EDGE('',*,*,#8276,.F.);
#10968=ORIENTED_EDGE('',*,*,#8277,.F.);
#10969=ORIENTED_EDGE('',*,*,#8278,.T.);
#10970=ORIENTED_EDGE('',*,*,#8275,.F.);
#10971=ORIENTED_EDGE('',*,*,#8279,.T.);
#10972=ORIENTED_EDGE('',*,*,#8280,.F.);
#10973=ORIENTED_EDGE('',*,*,#8281,.F.);
#10974=ORIENTED_EDGE('',*,*,#8267,.F.);
#10975=ORIENTED_EDGE('',*,*,#8274,.F.);
#10976=ORIENTED_EDGE('',*,*,#8253,.T.);
#10977=ORIENTED_EDGE('',*,*,#8282,.F.);
#10978=ORIENTED_EDGE('',*,*,#8279,.F.);
#10979=ORIENTED_EDGE('',*,*,#8283,.T.);
#10980=ORIENTED_EDGE('',*,*,#8124,.T.);
#10981=ORIENTED_EDGE('',*,*,#8284,.T.);
#10982=ORIENTED_EDGE('',*,*,#8285,.T.);
#10983=ORIENTED_EDGE('',*,*,#8286,.T.);
#10984=ORIENTED_EDGE('',*,*,#8125,.T.);
#10985=ORIENTED_EDGE('',*,*,#8283,.F.);
#10986=ORIENTED_EDGE('',*,*,#8287,.T.);
#10987=ORIENTED_EDGE('',*,*,#8288,.T.);
#10988=ORIENTED_EDGE('',*,*,#8126,.T.);
#10989=ORIENTED_EDGE('',*,*,#8286,.F.);
#10990=ORIENTED_EDGE('',*,*,#8289,.T.);
#10991=ORIENTED_EDGE('',*,*,#8288,.F.);
#10992=ORIENTED_EDGE('',*,*,#8290,.T.);
#10993=ORIENTED_EDGE('',*,*,#8291,.T.);
#10994=ORIENTED_EDGE('',*,*,#8284,.F.);
#10995=ORIENTED_EDGE('',*,*,#8292,.T.);
#10996=ORIENTED_EDGE('',*,*,#8293,.T.);
#10997=ORIENTED_EDGE('',*,*,#8291,.F.);
#10998=ORIENTED_EDGE('',*,*,#8294,.T.);
#10999=ORIENTED_EDGE('',*,*,#8295,.T.);
#11000=ORIENTED_EDGE('',*,*,#8127,.T.);
#11001=ORIENTED_EDGE('',*,*,#8290,.F.);
#11002=ORIENTED_EDGE('',*,*,#8296,.T.);
#11003=ORIENTED_EDGE('',*,*,#8258,.F.);
#11004=ORIENTED_EDGE('',*,*,#8262,.T.);
#11005=ORIENTED_EDGE('',*,*,#8297,.T.);
#11006=ORIENTED_EDGE('',*,*,#8235,.F.);
#11007=ORIENTED_EDGE('',*,*,#8196,.T.);
#11008=ORIENTED_EDGE('',*,*,#8298,.F.);
#11009=ORIENTED_EDGE('',*,*,#8299,.F.);
#11010=ORIENTED_EDGE('',*,*,#8259,.F.);
#11011=ORIENTED_EDGE('',*,*,#8296,.F.);
#11012=ORIENTED_EDGE('',*,*,#8289,.F.);
#11013=ORIENTED_EDGE('',*,*,#8300,.F.);
#11014=ORIENTED_EDGE('',*,*,#8234,.F.);
#11015=ORIENTED_EDGE('',*,*,#8300,.T.);
#11016=ORIENTED_EDGE('',*,*,#8287,.F.);
#11017=ORIENTED_EDGE('',*,*,#8301,.F.);
#11018=ORIENTED_EDGE('',*,*,#8232,.F.);
#11019=ORIENTED_EDGE('',*,*,#8301,.T.);
#11020=ORIENTED_EDGE('',*,*,#8285,.F.);
#11021=ORIENTED_EDGE('',*,*,#8302,.F.);
#11022=ORIENTED_EDGE('',*,*,#8241,.F.);
#11023=ORIENTED_EDGE('',*,*,#8214,.T.);
#11024=ORIENTED_EDGE('',*,*,#8209,.F.);
#11025=ORIENTED_EDGE('',*,*,#8137,.T.);
#11026=ORIENTED_EDGE('',*,*,#8114,.F.);
#11027=ORIENTED_EDGE('',*,*,#8303,.T.);
#11028=ORIENTED_EDGE('',*,*,#8304,.T.);
#11029=ORIENTED_EDGE('',*,*,#8019,.F.);
#11030=ORIENTED_EDGE('',*,*,#8304,.F.);
#11031=ORIENTED_EDGE('',*,*,#8305,.F.);
#11032=ORIENTED_EDGE('',*,*,#8255,.F.);
#11033=ORIENTED_EDGE('',*,*,#8212,.F.);
#11034=ORIENTED_EDGE('',*,*,#8306,.T.);
#11035=ORIENTED_EDGE('',*,*,#8129,.T.);
#11036=ORIENTED_EDGE('',*,*,#8307,.T.);
#11037=ORIENTED_EDGE('',*,*,#8195,.T.);
#11038=ORIENTED_EDGE('',*,*,#8197,.F.);
#11039=ORIENTED_EDGE('',*,*,#8198,.T.);
#11040=ORIENTED_EDGE('',*,*,#8306,.F.);
#11041=ORIENTED_EDGE('',*,*,#8095,.F.);
#11042=ORIENTED_EDGE('',*,*,#8308,.T.);
#11043=ORIENTED_EDGE('',*,*,#8292,.F.);
#11044=ORIENTED_EDGE('',*,*,#8123,.T.);
#11045=ORIENTED_EDGE('',*,*,#8093,.F.);
#11046=ORIENTED_EDGE('',*,*,#8081,.F.);
#11047=ORIENTED_EDGE('',*,*,#8078,.F.);
#11048=ORIENTED_EDGE('',*,*,#8087,.F.);
#11049=ORIENTED_EDGE('',*,*,#8293,.F.);
#11050=ORIENTED_EDGE('',*,*,#8309,.T.);
#11051=ORIENTED_EDGE('',*,*,#8244,.T.);
#11052=ORIENTED_EDGE('',*,*,#8242,.F.);
#11053=ORIENTED_EDGE('',*,*,#8302,.T.);
#11054=ORIENTED_EDGE('',*,*,#8119,.F.);
#11055=ORIENTED_EDGE('',*,*,#8310,.T.);
#11056=ORIENTED_EDGE('',*,*,#8311,.F.);
#11057=ORIENTED_EDGE('',*,*,#8247,.F.);
#11058=ORIENTED_EDGE('',*,*,#8305,.T.);
#11059=ORIENTED_EDGE('',*,*,#8303,.F.);
#11060=ORIENTED_EDGE('',*,*,#8113,.F.);
#11061=ORIENTED_EDGE('',*,*,#8117,.F.);
#11062=ORIENTED_EDGE('',*,*,#8109,.F.);
#11063=ORIENTED_EDGE('',*,*,#8106,.F.);
#11064=ORIENTED_EDGE('',*,*,#8105,.F.);
#11065=ORIENTED_EDGE('',*,*,#8310,.F.);
#11066=ORIENTED_EDGE('',*,*,#8122,.F.);
#11067=ORIENTED_EDGE('',*,*,#8312,.F.);
#11068=ORIENTED_EDGE('',*,*,#8313,.T.);
#11069=ORIENTED_EDGE('',*,*,#8314,.F.);
#11070=ORIENTED_EDGE('',*,*,#8315,.F.);
#11071=ORIENTED_EDGE('',*,*,#8316,.F.);
#11072=ORIENTED_EDGE('',*,*,#8317,.F.);
#11073=ORIENTED_EDGE('',*,*,#8318,.F.);
#11074=ORIENTED_EDGE('',*,*,#8319,.F.);
#11075=ORIENTED_EDGE('',*,*,#8320,.F.);
#11076=ORIENTED_EDGE('',*,*,#8121,.F.);
#11077=ORIENTED_EDGE('',*,*,#8321,.F.);
#11078=ORIENTED_EDGE('',*,*,#8322,.T.);
#11079=ORIENTED_EDGE('',*,*,#8134,.T.);
#11080=ORIENTED_EDGE('',*,*,#8318,.T.);
#11081=ORIENTED_EDGE('',*,*,#8280,.T.);
#11082=ORIENTED_EDGE('',*,*,#8323,.T.);
#11083=ORIENTED_EDGE('',*,*,#8135,.T.);
#11084=ORIENTED_EDGE('',*,*,#8322,.F.);
#11085=ORIENTED_EDGE('',*,*,#8282,.T.);
#11086=ORIENTED_EDGE('',*,*,#8321,.T.);
#11087=ORIENTED_EDGE('',*,*,#8136,.T.);
#11088=ORIENTED_EDGE('',*,*,#8323,.F.);
#11089=ORIENTED_EDGE('',*,*,#8252,.T.);
#11090=ORIENTED_EDGE('',*,*,#8324,.T.);
#11091=ORIENTED_EDGE('',*,*,#8312,.T.);
#11092=ORIENTED_EDGE('',*,*,#8320,.T.);
#11093=ORIENTED_EDGE('',*,*,#8251,.T.);
#11094=ORIENTED_EDGE('',*,*,#8249,.F.);
#11095=ORIENTED_EDGE('',*,*,#8319,.T.);
#11096=ORIENTED_EDGE('',*,*,#8133,.T.);
#11097=ORIENTED_EDGE('',*,*,#8315,.T.);
#11098=ORIENTED_EDGE('',*,*,#8325,.T.);
#11099=ORIENTED_EDGE('',*,*,#8268,.T.);
#11100=ORIENTED_EDGE('',*,*,#8264,.F.);
#11101=ORIENTED_EDGE('',*,*,#8281,.T.);
#11102=ORIENTED_EDGE('',*,*,#8317,.T.);
#11103=ORIENTED_EDGE('',*,*,#8326,.T.);
#11104=ORIENTED_EDGE('',*,*,#8277,.T.);
#11105=ORIENTED_EDGE('',*,*,#8316,.T.);
#11106=ORIENTED_EDGE('',*,*,#8132,.T.);
#11107=ORIENTED_EDGE('',*,*,#8192,.F.);
#11108=ORIENTED_EDGE('',*,*,#8270,.T.);
#11109=ORIENTED_EDGE('',*,*,#8327,.T.);
#11110=ORIENTED_EDGE('',*,*,#8314,.T.);
#11111=ORIENTED_EDGE('',*,*,#8276,.T.);
#11112=ORIENTED_EDGE('',*,*,#8266,.F.);
#11113=ORIENTED_EDGE('',*,*,#8326,.F.);
#11114=ORIENTED_EDGE('',*,*,#8325,.F.);
#11115=ORIENTED_EDGE('',*,*,#8327,.F.);
#11116=ORIENTED_EDGE('',*,*,#8269,.T.);
#11117=ORIENTED_EDGE('',*,*,#8328,.F.);
#11118=ORIENTED_EDGE('',*,*,#8329,.F.);
#11119=ORIENTED_EDGE('',*,*,#8295,.F.);
#11120=ORIENTED_EDGE('',*,*,#8128,.T.);
#11121=ORIENTED_EDGE('',*,*,#8329,.T.);
#11122=ORIENTED_EDGE('',*,*,#8298,.T.);
#11123=ORIENTED_EDGE('',*,*,#8307,.F.);
#11124=ORIENTED_EDGE('',*,*,#8260,.T.);
#11125=ORIENTED_EDGE('',*,*,#8256,.F.);
#11126=ORIENTED_EDGE('',*,*,#8299,.T.);
#11127=ORIENTED_EDGE('',*,*,#8328,.T.);
#11128=ORIENTED_EDGE('',*,*,#8330,.T.);
#11129=ORIENTED_EDGE('',*,*,#8263,.F.);
#11130=ORIENTED_EDGE('',*,*,#8331,.T.);
#11131=ORIENTED_EDGE('',*,*,#8225,.F.);
#11132=ORIENTED_EDGE('',*,*,#8331,.F.);
#11133=ORIENTED_EDGE('',*,*,#8332,.F.);
#11134=ORIENTED_EDGE('',*,*,#8333,.T.);
#11135=ORIENTED_EDGE('',*,*,#8224,.F.);
#11136=ORIENTED_EDGE('',*,*,#8333,.F.);
#11137=ORIENTED_EDGE('',*,*,#8271,.F.);
#11138=ORIENTED_EDGE('',*,*,#8334,.T.);
#11139=ORIENTED_EDGE('',*,*,#8223,.F.);
#11140=ORIENTED_EDGE('',*,*,#8334,.F.);
#11141=ORIENTED_EDGE('',*,*,#8246,.F.);
#11142=ORIENTED_EDGE('',*,*,#8335,.T.);
#11143=ORIENTED_EDGE('',*,*,#8222,.F.);
#11144=ORIENTED_EDGE('',*,*,#8335,.F.);
#11145=ORIENTED_EDGE('',*,*,#8297,.F.);
#11146=ORIENTED_EDGE('',*,*,#8261,.T.);
#11147=ORIENTED_EDGE('',*,*,#8330,.F.);
#11148=ORIENTED_EDGE('',*,*,#8294,.F.);
#11149=ORIENTED_EDGE('',*,*,#8248,.F.);
#11150=ORIENTED_EDGE('',*,*,#8311,.T.);
#11151=ORIENTED_EDGE('',*,*,#8313,.F.);
#11152=ORIENTED_EDGE('',*,*,#8324,.F.);
#11153=ORIENTED_EDGE('',*,*,#8332,.T.);
#11154=ORIENTED_EDGE('',*,*,#8100,.F.);
#11155=ORIENTED_EDGE('',*,*,#8245,.T.);
#11156=ORIENTED_EDGE('',*,*,#8309,.F.);
#11157=ORIENTED_EDGE('',*,*,#8308,.F.);
#11158=ORIENTED_EDGE('',*,*,#8022,.F.);
#11159=ORIENTED_EDGE('',*,*,#8045,.F.);
#11160=ORIENTED_EDGE('',*,*,#7991,.F.);
#11161=ORIENTED_EDGE('',*,*,#8076,.F.);
#11162=ORIENTED_EDGE('',*,*,#7954,.F.);
#11163=ORIENTED_EDGE('',*,*,#8151,.F.);
#11164=ORIENTED_EDGE('',*,*,#8155,.F.);
#11165=ORIENTED_EDGE('',*,*,#8159,.F.);
#11166=ORIENTED_EDGE('',*,*,#8163,.F.);
#11167=ORIENTED_EDGE('',*,*,#8168,.F.);
#11168=ORIENTED_EDGE('',*,*,#8240,.F.);
#11169=ORIENTED_EDGE('',*,*,#8336,.T.);
#11170=ORIENTED_EDGE('',*,*,#8337,.T.);
#11171=ORIENTED_EDGE('',*,*,#8336,.F.);
#11172=ORIENTED_EDGE('',*,*,#8337,.F.);
#11173=ORIENTED_EDGE('',*,*,#8338,.T.);
#11174=ORIENTED_EDGE('',*,*,#8338,.F.);
#11175=ORIENTED_EDGE('',*,*,#8339,.T.);
#11176=ORIENTED_EDGE('',*,*,#7938,.T.);
#11177=ORIENTED_EDGE('',*,*,#8339,.F.);
#11178=ORIENTED_EDGE('',*,*,#7940,.F.);
#11179=ORIENTED_EDGE('',*,*,#8185,.F.);
#11180=ORIENTED_EDGE('',*,*,#8278,.F.);
#11181=ORIENTED_EDGE('',*,*,#8191,.F.);
#11182=ORIENTED_EDGE('',*,*,#8188,.F.);
#11183=ORIENTED_EDGE('',*,*,#8340,.T.);
#11184=ORIENTED_EDGE('',*,*,#8341,.T.);
#11185=ORIENTED_EDGE('',*,*,#8342,.T.);
#11186=ORIENTED_EDGE('',*,*,#8343,.T.);
#11187=ORIENTED_EDGE('',*,*,#8341,.F.);
#11188=ORIENTED_EDGE('',*,*,#8344,.T.);
#11189=ORIENTED_EDGE('',*,*,#8345,.F.);
#11190=ORIENTED_EDGE('',*,*,#8346,.T.);
#11191=ORIENTED_EDGE('',*,*,#8340,.F.);
#11192=ORIENTED_EDGE('',*,*,#8347,.F.);
#11193=ORIENTED_EDGE('',*,*,#8348,.F.);
#11194=ORIENTED_EDGE('',*,*,#8349,.F.);
#11195=ORIENTED_EDGE('',*,*,#8350,.F.);
#11196=ORIENTED_EDGE('',*,*,#8351,.F.);
#11197=ORIENTED_EDGE('',*,*,#8352,.F.);
#11198=ORIENTED_EDGE('',*,*,#8344,.F.);
#11199=ORIENTED_EDGE('',*,*,#8353,.T.);
#11200=ORIENTED_EDGE('',*,*,#8345,.T.);
#11201=ORIENTED_EDGE('',*,*,#8352,.T.);
#11202=ORIENTED_EDGE('',*,*,#8354,.T.);
#11203=ORIENTED_EDGE('',*,*,#8354,.F.);
#11204=ORIENTED_EDGE('',*,*,#8351,.T.);
#11205=ORIENTED_EDGE('',*,*,#8355,.F.);
#11206=ORIENTED_EDGE('',*,*,#8356,.T.);
#11207=ORIENTED_EDGE('',*,*,#8357,.T.);
#11208=ORIENTED_EDGE('',*,*,#8358,.T.);
#11209=ORIENTED_EDGE('',*,*,#8359,.T.);
#11210=ORIENTED_EDGE('',*,*,#8348,.T.);
#11211=ORIENTED_EDGE('',*,*,#8360,.T.);
#11212=ORIENTED_EDGE('',*,*,#8343,.F.);
#11213=ORIENTED_EDGE('',*,*,#8361,.T.);
#11214=ORIENTED_EDGE('',*,*,#8360,.F.);
#11215=ORIENTED_EDGE('',*,*,#8347,.T.);
#11216=ORIENTED_EDGE('',*,*,#8362,.T.);
#11217=ORIENTED_EDGE('',*,*,#8350,.T.);
#11218=ORIENTED_EDGE('',*,*,#8363,.T.);
#11219=ORIENTED_EDGE('',*,*,#8364,.T.);
#11220=ORIENTED_EDGE('',*,*,#8355,.T.);
#11221=ORIENTED_EDGE('',*,*,#8342,.F.);
#11222=ORIENTED_EDGE('',*,*,#8346,.F.);
#11223=ORIENTED_EDGE('',*,*,#8353,.F.);
#11224=ORIENTED_EDGE('',*,*,#8356,.F.);
#11225=ORIENTED_EDGE('',*,*,#8364,.F.);
#11226=ORIENTED_EDGE('',*,*,#8365,.F.);
#11227=ORIENTED_EDGE('',*,*,#8358,.F.);
#11228=ORIENTED_EDGE('',*,*,#8361,.F.);
#11229=ORIENTED_EDGE('',*,*,#8362,.F.);
#11230=ORIENTED_EDGE('',*,*,#8366,.T.);
#11231=ORIENTED_EDGE('',*,*,#8357,.F.);
#11232=ORIENTED_EDGE('',*,*,#8366,.F.);
#11233=ORIENTED_EDGE('',*,*,#8359,.F.);
#11234=ORIENTED_EDGE('',*,*,#8365,.T.);
#11235=ORIENTED_EDGE('',*,*,#8363,.F.);
#11236=ORIENTED_EDGE('',*,*,#8349,.T.);
#11237=ORIENTED_EDGE('',*,*,#8367,.T.);
#11238=ORIENTED_EDGE('',*,*,#8368,.T.);
#11239=ORIENTED_EDGE('',*,*,#8369,.T.);
#11240=ORIENTED_EDGE('',*,*,#8370,.T.);
#11241=ORIENTED_EDGE('',*,*,#8369,.F.);
#11242=ORIENTED_EDGE('',*,*,#8370,.F.);
#11243=ORIENTED_EDGE('',*,*,#8371,.T.);
#11244=ORIENTED_EDGE('',*,*,#8372,.T.);
#11245=ORIENTED_EDGE('',*,*,#8373,.T.);
#11246=ORIENTED_EDGE('',*,*,#8374,.T.);
#11247=ORIENTED_EDGE('',*,*,#8375,.T.);
#11248=ORIENTED_EDGE('',*,*,#8376,.T.);
#11249=ORIENTED_EDGE('',*,*,#8377,.T.);
#11250=ORIENTED_EDGE('',*,*,#8378,.F.);
#11251=ORIENTED_EDGE('',*,*,#8379,.T.);
#11252=ORIENTED_EDGE('',*,*,#8380,.F.);
#11253=ORIENTED_EDGE('',*,*,#8381,.F.);
#11254=ORIENTED_EDGE('',*,*,#8382,.F.);
#11255=ORIENTED_EDGE('',*,*,#8383,.T.);
#11256=ORIENTED_EDGE('',*,*,#8367,.F.);
#11257=ORIENTED_EDGE('',*,*,#8368,.F.);
#11258=ORIENTED_EDGE('',*,*,#8383,.F.);
#11259=ORIENTED_EDGE('',*,*,#8384,.T.);
#11260=ORIENTED_EDGE('',*,*,#8385,.T.);
#11261=ORIENTED_EDGE('',*,*,#8378,.T.);
#11262=ORIENTED_EDGE('',*,*,#8386,.T.);
#11263=ORIENTED_EDGE('',*,*,#8380,.T.);
#11264=ORIENTED_EDGE('',*,*,#8387,.T.);
#11265=ORIENTED_EDGE('',*,*,#8388,.T.);
#11266=ORIENTED_EDGE('',*,*,#8389,.T.);
#11267=ORIENTED_EDGE('',*,*,#8381,.T.);
#11268=ORIENTED_EDGE('',*,*,#8389,.F.);
#11269=ORIENTED_EDGE('',*,*,#8390,.T.);
#11270=ORIENTED_EDGE('',*,*,#8386,.F.);
#11271=ORIENTED_EDGE('',*,*,#8384,.F.);
#11272=ORIENTED_EDGE('',*,*,#8391,.T.);
#11273=ORIENTED_EDGE('',*,*,#8392,.F.);
#11274=ORIENTED_EDGE('',*,*,#8393,.F.);
#11275=ORIENTED_EDGE('',*,*,#8390,.F.);
#11276=ORIENTED_EDGE('',*,*,#8394,.F.);
#11277=ORIENTED_EDGE('',*,*,#8395,.F.);
#11278=ORIENTED_EDGE('',*,*,#8391,.F.);
#11279=ORIENTED_EDGE('',*,*,#8385,.F.);
#11280=ORIENTED_EDGE('',*,*,#8393,.T.);
#11281=ORIENTED_EDGE('',*,*,#8396,.F.);
#11282=ORIENTED_EDGE('',*,*,#8397,.T.);
#11283=ORIENTED_EDGE('',*,*,#8398,.F.);
#11284=ORIENTED_EDGE('',*,*,#8399,.T.);
#11285=ORIENTED_EDGE('',*,*,#8387,.F.);
#11286=ORIENTED_EDGE('',*,*,#8379,.F.);
#11287=ORIENTED_EDGE('',*,*,#8388,.F.);
#11288=ORIENTED_EDGE('',*,*,#8399,.F.);
#11289=ORIENTED_EDGE('',*,*,#8400,.F.);
#11290=ORIENTED_EDGE('',*,*,#8394,.T.);
#11291=ORIENTED_EDGE('',*,*,#8401,.T.);
#11292=ORIENTED_EDGE('',*,*,#8396,.T.);
#11293=ORIENTED_EDGE('',*,*,#8392,.T.);
#11294=ORIENTED_EDGE('',*,*,#8402,.T.);
#11295=ORIENTED_EDGE('',*,*,#8400,.T.);
#11296=ORIENTED_EDGE('',*,*,#8398,.T.);
#11297=ORIENTED_EDGE('',*,*,#8403,.T.);
#11298=ORIENTED_EDGE('',*,*,#8404,.T.);
#11299=ORIENTED_EDGE('',*,*,#8395,.T.);
#11300=ORIENTED_EDGE('',*,*,#8404,.F.);
#11301=ORIENTED_EDGE('',*,*,#8405,.T.);
#11302=ORIENTED_EDGE('',*,*,#8402,.F.);
#11303=ORIENTED_EDGE('',*,*,#8406,.T.);
#11304=ORIENTED_EDGE('',*,*,#8401,.F.);
#11305=ORIENTED_EDGE('',*,*,#8405,.F.);
#11306=ORIENTED_EDGE('',*,*,#8403,.F.);
#11307=ORIENTED_EDGE('',*,*,#8397,.F.);
#11308=ORIENTED_EDGE('',*,*,#8407,.T.);
#11309=ORIENTED_EDGE('',*,*,#8408,.T.);
#11310=ORIENTED_EDGE('',*,*,#8409,.T.);
#11311=ORIENTED_EDGE('',*,*,#8410,.T.);
#11312=ORIENTED_EDGE('',*,*,#8411,.T.);
#11313=ORIENTED_EDGE('',*,*,#8412,.T.);
#11314=ORIENTED_EDGE('',*,*,#8413,.T.);
#11315=ORIENTED_EDGE('',*,*,#8413,.F.);
#11316=ORIENTED_EDGE('',*,*,#8414,.T.);
#11317=ORIENTED_EDGE('',*,*,#8415,.F.);
#11318=ORIENTED_EDGE('',*,*,#8414,.F.);
#11319=ORIENTED_EDGE('',*,*,#8377,.F.);
#11320=ORIENTED_EDGE('',*,*,#8416,.T.);
#11321=ORIENTED_EDGE('',*,*,#8417,.T.);
#11322=ORIENTED_EDGE('',*,*,#8416,.F.);
#11323=ORIENTED_EDGE('',*,*,#8417,.F.);
#11324=ORIENTED_EDGE('',*,*,#8415,.T.);
#11325=ORIENTED_EDGE('',*,*,#8412,.F.);
#11326=ORIENTED_EDGE('',*,*,#8418,.T.);
#11327=ORIENTED_EDGE('',*,*,#8419,.F.);
#11328=ORIENTED_EDGE('',*,*,#8418,.F.);
#11329=ORIENTED_EDGE('',*,*,#8376,.F.);
#11330=ORIENTED_EDGE('',*,*,#8420,.T.);
#11331=ORIENTED_EDGE('',*,*,#8421,.T.);
#11332=ORIENTED_EDGE('',*,*,#8420,.F.);
#11333=ORIENTED_EDGE('',*,*,#8421,.F.);
#11334=ORIENTED_EDGE('',*,*,#8419,.T.);
#11335=ORIENTED_EDGE('',*,*,#8411,.F.);
#11336=ORIENTED_EDGE('',*,*,#8422,.T.);
#11337=ORIENTED_EDGE('',*,*,#8423,.F.);
#11338=ORIENTED_EDGE('',*,*,#8422,.F.);
#11339=ORIENTED_EDGE('',*,*,#8375,.F.);
#11340=ORIENTED_EDGE('',*,*,#8424,.T.);
#11341=ORIENTED_EDGE('',*,*,#8425,.T.);
#11342=ORIENTED_EDGE('',*,*,#8424,.F.);
#11343=ORIENTED_EDGE('',*,*,#8425,.F.);
#11344=ORIENTED_EDGE('',*,*,#8423,.T.);
#11345=ORIENTED_EDGE('',*,*,#8410,.F.);
#11346=ORIENTED_EDGE('',*,*,#8426,.T.);
#11347=ORIENTED_EDGE('',*,*,#8427,.F.);
#11348=ORIENTED_EDGE('',*,*,#8426,.F.);
#11349=ORIENTED_EDGE('',*,*,#8374,.F.);
#11350=ORIENTED_EDGE('',*,*,#8428,.T.);
#11351=ORIENTED_EDGE('',*,*,#8429,.T.);
#11352=ORIENTED_EDGE('',*,*,#8428,.F.);
#11353=ORIENTED_EDGE('',*,*,#8429,.F.);
#11354=ORIENTED_EDGE('',*,*,#8427,.T.);
#11355=ORIENTED_EDGE('',*,*,#8409,.F.);
#11356=ORIENTED_EDGE('',*,*,#8430,.T.);
#11357=ORIENTED_EDGE('',*,*,#8431,.F.);
#11358=ORIENTED_EDGE('',*,*,#8430,.F.);
#11359=ORIENTED_EDGE('',*,*,#8373,.F.);
#11360=ORIENTED_EDGE('',*,*,#8432,.T.);
#11361=ORIENTED_EDGE('',*,*,#8433,.T.);
#11362=ORIENTED_EDGE('',*,*,#8432,.F.);
#11363=ORIENTED_EDGE('',*,*,#8433,.F.);
#11364=ORIENTED_EDGE('',*,*,#8431,.T.);
#11365=ORIENTED_EDGE('',*,*,#8408,.F.);
#11366=ORIENTED_EDGE('',*,*,#8434,.T.);
#11367=ORIENTED_EDGE('',*,*,#8435,.F.);
#11368=ORIENTED_EDGE('',*,*,#8434,.F.);
#11369=ORIENTED_EDGE('',*,*,#8372,.F.);
#11370=ORIENTED_EDGE('',*,*,#8436,.T.);
#11371=ORIENTED_EDGE('',*,*,#8437,.T.);
#11372=ORIENTED_EDGE('',*,*,#8436,.F.);
#11373=ORIENTED_EDGE('',*,*,#8437,.F.);
#11374=ORIENTED_EDGE('',*,*,#8435,.T.);
#11375=ORIENTED_EDGE('',*,*,#8407,.F.);
#11376=ORIENTED_EDGE('',*,*,#8438,.T.);
#11377=ORIENTED_EDGE('',*,*,#8439,.F.);
#11378=ORIENTED_EDGE('',*,*,#8438,.F.);
#11379=ORIENTED_EDGE('',*,*,#8371,.F.);
#11380=ORIENTED_EDGE('',*,*,#8440,.T.);
#11381=ORIENTED_EDGE('',*,*,#8441,.T.);
#11382=ORIENTED_EDGE('',*,*,#8440,.F.);
#11383=ORIENTED_EDGE('',*,*,#8441,.F.);
#11384=ORIENTED_EDGE('',*,*,#8439,.T.);
#11385=ORIENTED_EDGE('',*,*,#8406,.F.);
#11386=ORIENTED_EDGE('',*,*,#8442,.T.);
#11387=ORIENTED_EDGE('',*,*,#8382,.T.);
#11388=ORIENTED_EDGE('',*,*,#8442,.F.);
#11389=ORIENTED_EDGE('',*,*,#8443,.T.);
#11390=ORIENTED_EDGE('',*,*,#8444,.T.);
#11391=ORIENTED_EDGE('',*,*,#8445,.T.);
#11392=ORIENTED_EDGE('',*,*,#8446,.T.);
#11393=ORIENTED_EDGE('',*,*,#8444,.F.);
#11394=ORIENTED_EDGE('',*,*,#8447,.F.);
#11395=ORIENTED_EDGE('',*,*,#8448,.F.);
#11396=ORIENTED_EDGE('',*,*,#8449,.T.);
#11397=ORIENTED_EDGE('',*,*,#8450,.T.);
#11398=ORIENTED_EDGE('',*,*,#8448,.T.);
#11399=ORIENTED_EDGE('',*,*,#8451,.T.);
#11400=ORIENTED_EDGE('',*,*,#8452,.T.);
#11401=ORIENTED_EDGE('',*,*,#8453,.T.);
#11402=ORIENTED_EDGE('',*,*,#8454,.T.);
#11403=ORIENTED_EDGE('',*,*,#8455,.T.);
#11404=ORIENTED_EDGE('',*,*,#8456,.T.);
#11405=ORIENTED_EDGE('',*,*,#8454,.F.);
#11406=ORIENTED_EDGE('',*,*,#8457,.F.);
#11407=ORIENTED_EDGE('',*,*,#8458,.F.);
#11408=ORIENTED_EDGE('',*,*,#8459,.T.);
#11409=ORIENTED_EDGE('',*,*,#8460,.T.);
#11410=ORIENTED_EDGE('',*,*,#8458,.T.);
#11411=ORIENTED_EDGE('',*,*,#8461,.T.);
#11412=ORIENTED_EDGE('',*,*,#8462,.T.);
#11413=ORIENTED_EDGE('',*,*,#8463,.T.);
#11414=ORIENTED_EDGE('',*,*,#8464,.T.);
#11415=ORIENTED_EDGE('',*,*,#8465,.T.);
#11416=ORIENTED_EDGE('',*,*,#8466,.T.);
#11417=ORIENTED_EDGE('',*,*,#8464,.F.);
#11418=ORIENTED_EDGE('',*,*,#8467,.F.);
#11419=ORIENTED_EDGE('',*,*,#8468,.F.);
#11420=ORIENTED_EDGE('',*,*,#8469,.T.);
#11421=ORIENTED_EDGE('',*,*,#8470,.T.);
#11422=ORIENTED_EDGE('',*,*,#8468,.T.);
#11423=ORIENTED_EDGE('',*,*,#8471,.T.);
#11424=ORIENTED_EDGE('',*,*,#8472,.T.);
#11425=ORIENTED_EDGE('',*,*,#8473,.T.);
#11426=ORIENTED_EDGE('',*,*,#8474,.T.);
#11427=ORIENTED_EDGE('',*,*,#8475,.T.);
#11428=ORIENTED_EDGE('',*,*,#8476,.T.);
#11429=ORIENTED_EDGE('',*,*,#8474,.F.);
#11430=ORIENTED_EDGE('',*,*,#8477,.F.);
#11431=ORIENTED_EDGE('',*,*,#8478,.F.);
#11432=ORIENTED_EDGE('',*,*,#8479,.T.);
#11433=ORIENTED_EDGE('',*,*,#8480,.T.);
#11434=ORIENTED_EDGE('',*,*,#8478,.T.);
#11435=ORIENTED_EDGE('',*,*,#8481,.T.);
#11436=ORIENTED_EDGE('',*,*,#8482,.T.);
#11437=ORIENTED_EDGE('',*,*,#8483,.F.);
#11438=ORIENTED_EDGE('',*,*,#8481,.F.);
#11439=ORIENTED_EDGE('',*,*,#8477,.T.);
#11440=ORIENTED_EDGE('',*,*,#8473,.F.);
#11441=ORIENTED_EDGE('',*,*,#8484,.F.);
#11442=ORIENTED_EDGE('',*,*,#8465,.F.);
#11443=ORIENTED_EDGE('',*,*,#8469,.F.);
#11444=ORIENTED_EDGE('',*,*,#8470,.F.);
#11445=ORIENTED_EDGE('',*,*,#8485,.F.);
#11446=ORIENTED_EDGE('',*,*,#8471,.F.);
#11447=ORIENTED_EDGE('',*,*,#8467,.T.);
#11448=ORIENTED_EDGE('',*,*,#8463,.F.);
#11449=ORIENTED_EDGE('',*,*,#8486,.F.);
#11450=ORIENTED_EDGE('',*,*,#8475,.F.);
#11451=ORIENTED_EDGE('',*,*,#8479,.F.);
#11452=ORIENTED_EDGE('',*,*,#8480,.F.);
#11453=ORIENTED_EDGE('',*,*,#8487,.F.);
#11454=ORIENTED_EDGE('',*,*,#8461,.F.);
#11455=ORIENTED_EDGE('',*,*,#8457,.T.);
#11456=ORIENTED_EDGE('',*,*,#8453,.F.);
#11457=ORIENTED_EDGE('',*,*,#8488,.F.);
#11458=ORIENTED_EDGE('',*,*,#8445,.F.);
#11459=ORIENTED_EDGE('',*,*,#8449,.F.);
#11460=ORIENTED_EDGE('',*,*,#8450,.F.);
#11461=ORIENTED_EDGE('',*,*,#8489,.F.);
#11462=ORIENTED_EDGE('',*,*,#8451,.F.);
#11463=ORIENTED_EDGE('',*,*,#8447,.T.);
#11464=ORIENTED_EDGE('',*,*,#8443,.F.);
#11465=ORIENTED_EDGE('',*,*,#8490,.F.);
#11466=ORIENTED_EDGE('',*,*,#8455,.F.);
#11467=ORIENTED_EDGE('',*,*,#8459,.F.);
#11468=ORIENTED_EDGE('',*,*,#8460,.F.);
#11469=ORIENTED_EDGE('',*,*,#8491,.T.);
#11470=ORIENTED_EDGE('',*,*,#8492,.T.);
#11471=ORIENTED_EDGE('',*,*,#8493,.F.);
#11472=ORIENTED_EDGE('',*,*,#8492,.F.);
#11473=ORIENTED_EDGE('',*,*,#8494,.F.);
#11474=ORIENTED_EDGE('',*,*,#8489,.T.);
#11475=ORIENTED_EDGE('',*,*,#8462,.F.);
#11476=ORIENTED_EDGE('',*,*,#8487,.T.);
#11477=ORIENTED_EDGE('',*,*,#8452,.F.);
#11478=ORIENTED_EDGE('',*,*,#8485,.T.);
#11479=ORIENTED_EDGE('',*,*,#8482,.F.);
#11480=ORIENTED_EDGE('',*,*,#8483,.T.);
#11481=ORIENTED_EDGE('',*,*,#8472,.F.);
#11482=ORIENTED_EDGE('',*,*,#8493,.T.);
#11483=ORIENTED_EDGE('',*,*,#8495,.F.);
#11484=ORIENTED_EDGE('',*,*,#8496,.T.);
#11485=ORIENTED_EDGE('',*,*,#8494,.T.);
#11486=ORIENTED_EDGE('',*,*,#8496,.F.);
#11487=ORIENTED_EDGE('',*,*,#8495,.T.);
#11488=ORIENTED_EDGE('',*,*,#8488,.T.);
#11489=ORIENTED_EDGE('',*,*,#8456,.F.);
#11490=ORIENTED_EDGE('',*,*,#8490,.T.);
#11491=ORIENTED_EDGE('',*,*,#8446,.F.);
#11492=ORIENTED_EDGE('',*,*,#8484,.T.);
#11493=ORIENTED_EDGE('',*,*,#8476,.F.);
#11494=ORIENTED_EDGE('',*,*,#8486,.T.);
#11495=ORIENTED_EDGE('',*,*,#8466,.F.);
#11496=ORIENTED_EDGE('',*,*,#8491,.F.);
#11497=ORIENTED_EDGE('',*,*,#8497,.T.);
#11498=ORIENTED_EDGE('',*,*,#8498,.T.);
#11499=ORIENTED_EDGE('',*,*,#8499,.T.);
#11500=ORIENTED_EDGE('',*,*,#8500,.T.);
#11501=ORIENTED_EDGE('',*,*,#8501,.T.);
#11502=ORIENTED_EDGE('',*,*,#8502,.T.);
#11503=ORIENTED_EDGE('',*,*,#8503,.T.);
#11504=ORIENTED_EDGE('',*,*,#8504,.T.);
#11505=ORIENTED_EDGE('',*,*,#8505,.T.);
#11506=ORIENTED_EDGE('',*,*,#8504,.F.);
#11507=ORIENTED_EDGE('',*,*,#8506,.T.);
#11508=ORIENTED_EDGE('',*,*,#8507,.T.);
#11509=ORIENTED_EDGE('',*,*,#8508,.T.);
#11510=ORIENTED_EDGE('',*,*,#8500,.F.);
#11511=ORIENTED_EDGE('',*,*,#8497,.F.);
#11512=ORIENTED_EDGE('',*,*,#8508,.F.);
#11513=ORIENTED_EDGE('',*,*,#8509,.T.);
#11514=ORIENTED_EDGE('',*,*,#8510,.F.);
#11515=ORIENTED_EDGE('',*,*,#8511,.F.);
#11516=ORIENTED_EDGE('',*,*,#8512,.F.);
#11517=ORIENTED_EDGE('',*,*,#8513,.F.);
#11518=ORIENTED_EDGE('',*,*,#8507,.F.);
#11519=ORIENTED_EDGE('',*,*,#8514,.F.);
#11520=ORIENTED_EDGE('',*,*,#8515,.F.);
#11521=ORIENTED_EDGE('',*,*,#8509,.F.);
#11522=ORIENTED_EDGE('',*,*,#8503,.F.);
#11523=ORIENTED_EDGE('',*,*,#8516,.F.);
#11524=ORIENTED_EDGE('',*,*,#8517,.F.);
#11525=ORIENTED_EDGE('',*,*,#8518,.F.);
#11526=ORIENTED_EDGE('',*,*,#8519,.T.);
#11527=ORIENTED_EDGE('',*,*,#8514,.T.);
#11528=ORIENTED_EDGE('',*,*,#8506,.F.);
#11529=ORIENTED_EDGE('',*,*,#8520,.T.);
#11530=ORIENTED_EDGE('',*,*,#8521,.T.);
#11531=ORIENTED_EDGE('',*,*,#8522,.T.);
#11532=ORIENTED_EDGE('',*,*,#8523,.T.);
#11533=ORIENTED_EDGE('',*,*,#8524,.T.);
#11534=ORIENTED_EDGE('',*,*,#8525,.T.);
#11535=ORIENTED_EDGE('',*,*,#8526,.T.);
#11536=ORIENTED_EDGE('',*,*,#8527,.T.);
#11537=ORIENTED_EDGE('',*,*,#8528,.T.);
#11538=ORIENTED_EDGE('',*,*,#8527,.F.);
#11539=ORIENTED_EDGE('',*,*,#8529,.T.);
#11540=ORIENTED_EDGE('',*,*,#8530,.T.);
#11541=ORIENTED_EDGE('',*,*,#8531,.T.);
#11542=ORIENTED_EDGE('',*,*,#8523,.F.);
#11543=ORIENTED_EDGE('',*,*,#8520,.F.);
#11544=ORIENTED_EDGE('',*,*,#8531,.F.);
#11545=ORIENTED_EDGE('',*,*,#8532,.T.);
#11546=ORIENTED_EDGE('',*,*,#8533,.F.);
#11547=ORIENTED_EDGE('',*,*,#8534,.F.);
#11548=ORIENTED_EDGE('',*,*,#8535,.F.);
#11549=ORIENTED_EDGE('',*,*,#8536,.F.);
#11550=ORIENTED_EDGE('',*,*,#8530,.F.);
#11551=ORIENTED_EDGE('',*,*,#8537,.F.);
#11552=ORIENTED_EDGE('',*,*,#8538,.F.);
#11553=ORIENTED_EDGE('',*,*,#8532,.F.);
#11554=ORIENTED_EDGE('',*,*,#8526,.F.);
#11555=ORIENTED_EDGE('',*,*,#8539,.F.);
#11556=ORIENTED_EDGE('',*,*,#8540,.F.);
#11557=ORIENTED_EDGE('',*,*,#8541,.F.);
#11558=ORIENTED_EDGE('',*,*,#8542,.T.);
#11559=ORIENTED_EDGE('',*,*,#8537,.T.);
#11560=ORIENTED_EDGE('',*,*,#8529,.F.);
#11561=ORIENTED_EDGE('',*,*,#8543,.T.);
#11562=ORIENTED_EDGE('',*,*,#8544,.T.);
#11563=ORIENTED_EDGE('',*,*,#8545,.T.);
#11564=ORIENTED_EDGE('',*,*,#8546,.T.);
#11565=ORIENTED_EDGE('',*,*,#8547,.T.);
#11566=ORIENTED_EDGE('',*,*,#8548,.T.);
#11567=ORIENTED_EDGE('',*,*,#8549,.T.);
#11568=ORIENTED_EDGE('',*,*,#8550,.T.);
#11569=ORIENTED_EDGE('',*,*,#8551,.T.);
#11570=ORIENTED_EDGE('',*,*,#8550,.F.);
#11571=ORIENTED_EDGE('',*,*,#8552,.T.);
#11572=ORIENTED_EDGE('',*,*,#8553,.T.);
#11573=ORIENTED_EDGE('',*,*,#8554,.T.);
#11574=ORIENTED_EDGE('',*,*,#8546,.F.);
#11575=ORIENTED_EDGE('',*,*,#8543,.F.);
#11576=ORIENTED_EDGE('',*,*,#8554,.F.);
#11577=ORIENTED_EDGE('',*,*,#8555,.T.);
#11578=ORIENTED_EDGE('',*,*,#8556,.F.);
#11579=ORIENTED_EDGE('',*,*,#8557,.F.);
#11580=ORIENTED_EDGE('',*,*,#8558,.F.);
#11581=ORIENTED_EDGE('',*,*,#8559,.F.);
#11582=ORIENTED_EDGE('',*,*,#8553,.F.);
#11583=ORIENTED_EDGE('',*,*,#8560,.F.);
#11584=ORIENTED_EDGE('',*,*,#8561,.F.);
#11585=ORIENTED_EDGE('',*,*,#8555,.F.);
#11586=ORIENTED_EDGE('',*,*,#8549,.F.);
#11587=ORIENTED_EDGE('',*,*,#8562,.F.);
#11588=ORIENTED_EDGE('',*,*,#8563,.F.);
#11589=ORIENTED_EDGE('',*,*,#8564,.F.);
#11590=ORIENTED_EDGE('',*,*,#8565,.T.);
#11591=ORIENTED_EDGE('',*,*,#8560,.T.);
#11592=ORIENTED_EDGE('',*,*,#8552,.F.);
#11593=ORIENTED_EDGE('',*,*,#8566,.T.);
#11594=ORIENTED_EDGE('',*,*,#8567,.T.);
#11595=ORIENTED_EDGE('',*,*,#8568,.T.);
#11596=ORIENTED_EDGE('',*,*,#8569,.T.);
#11597=ORIENTED_EDGE('',*,*,#8570,.T.);
#11598=ORIENTED_EDGE('',*,*,#8571,.T.);
#11599=ORIENTED_EDGE('',*,*,#8572,.T.);
#11600=ORIENTED_EDGE('',*,*,#8573,.T.);
#11601=ORIENTED_EDGE('',*,*,#8574,.T.);
#11602=ORIENTED_EDGE('',*,*,#8573,.F.);
#11603=ORIENTED_EDGE('',*,*,#8575,.T.);
#11604=ORIENTED_EDGE('',*,*,#8576,.T.);
#11605=ORIENTED_EDGE('',*,*,#8577,.T.);
#11606=ORIENTED_EDGE('',*,*,#8569,.F.);
#11607=ORIENTED_EDGE('',*,*,#8566,.F.);
#11608=ORIENTED_EDGE('',*,*,#8577,.F.);
#11609=ORIENTED_EDGE('',*,*,#8578,.T.);
#11610=ORIENTED_EDGE('',*,*,#8579,.F.);
#11611=ORIENTED_EDGE('',*,*,#8580,.F.);
#11612=ORIENTED_EDGE('',*,*,#8581,.F.);
#11613=ORIENTED_EDGE('',*,*,#8582,.F.);
#11614=ORIENTED_EDGE('',*,*,#8576,.F.);
#11615=ORIENTED_EDGE('',*,*,#8583,.F.);
#11616=ORIENTED_EDGE('',*,*,#8584,.F.);
#11617=ORIENTED_EDGE('',*,*,#8578,.F.);
#11618=ORIENTED_EDGE('',*,*,#8572,.F.);
#11619=ORIENTED_EDGE('',*,*,#8585,.F.);
#11620=ORIENTED_EDGE('',*,*,#8586,.F.);
#11621=ORIENTED_EDGE('',*,*,#8587,.F.);
#11622=ORIENTED_EDGE('',*,*,#8588,.T.);
#11623=ORIENTED_EDGE('',*,*,#8583,.T.);
#11624=ORIENTED_EDGE('',*,*,#8575,.F.);
#11625=ORIENTED_EDGE('',*,*,#8589,.T.);
#11626=ORIENTED_EDGE('',*,*,#8590,.T.);
#11627=ORIENTED_EDGE('',*,*,#8591,.T.);
#11628=ORIENTED_EDGE('',*,*,#8592,.T.);
#11629=ORIENTED_EDGE('',*,*,#8592,.F.);
#11630=ORIENTED_EDGE('',*,*,#8593,.F.);
#11631=ORIENTED_EDGE('',*,*,#8594,.T.);
#11632=ORIENTED_EDGE('',*,*,#8595,.F.);
#11633=ORIENTED_EDGE('',*,*,#8596,.F.);
#11634=ORIENTED_EDGE('',*,*,#8597,.F.);
#11635=ORIENTED_EDGE('',*,*,#8598,.F.);
#11636=ORIENTED_EDGE('',*,*,#8599,.T.);
#11637=ORIENTED_EDGE('',*,*,#8600,.T.);
#11638=ORIENTED_EDGE('',*,*,#8601,.T.);
#11639=ORIENTED_EDGE('',*,*,#8602,.T.);
#11640=ORIENTED_EDGE('',*,*,#8603,.T.);
#11641=ORIENTED_EDGE('',*,*,#8593,.T.);
#11642=ORIENTED_EDGE('',*,*,#8591,.F.);
#11643=ORIENTED_EDGE('',*,*,#8604,.T.);
#11644=ORIENTED_EDGE('',*,*,#8602,.F.);
#11645=ORIENTED_EDGE('',*,*,#8605,.T.);
#11646=ORIENTED_EDGE('',*,*,#8601,.F.);
#11647=ORIENTED_EDGE('',*,*,#8606,.F.);
#11648=ORIENTED_EDGE('',*,*,#8607,.F.);
#11649=ORIENTED_EDGE('',*,*,#8608,.F.);
#11650=ORIENTED_EDGE('',*,*,#8609,.T.);
#11651=ORIENTED_EDGE('',*,*,#8610,.T.);
#11652=ORIENTED_EDGE('',*,*,#8605,.F.);
#11653=ORIENTED_EDGE('',*,*,#8600,.F.);
#11654=ORIENTED_EDGE('',*,*,#8611,.F.);
#11655=ORIENTED_EDGE('',*,*,#8612,.F.);
#11656=ORIENTED_EDGE('',*,*,#8613,.T.);
#11657=ORIENTED_EDGE('',*,*,#8614,.T.);
#11658=ORIENTED_EDGE('',*,*,#8606,.T.);
#11659=ORIENTED_EDGE('',*,*,#8615,.F.);
#11660=ORIENTED_EDGE('',*,*,#8616,.T.);
#11661=ORIENTED_EDGE('',*,*,#8617,.F.);
#11662=ORIENTED_EDGE('',*,*,#8618,.F.);
#11663=ORIENTED_EDGE('',*,*,#8619,.T.);
#11664=ORIENTED_EDGE('',*,*,#8620,.F.);
#11665=ORIENTED_EDGE('',*,*,#8621,.F.);
#11666=ORIENTED_EDGE('',*,*,#8622,.F.);
#11667=ORIENTED_EDGE('',*,*,#8623,.T.);
#11668=ORIENTED_EDGE('',*,*,#8624,.F.);
#11669=ORIENTED_EDGE('',*,*,#8625,.F.);
#11670=ORIENTED_EDGE('',*,*,#8626,.F.);
#11671=ORIENTED_EDGE('',*,*,#8627,.T.);
#11672=ORIENTED_EDGE('',*,*,#8628,.F.);
#11673=ORIENTED_EDGE('',*,*,#8629,.F.);
#11674=ORIENTED_EDGE('',*,*,#8630,.F.);
#11675=ORIENTED_EDGE('',*,*,#8611,.T.);
#11676=ORIENTED_EDGE('',*,*,#8599,.F.);
#11677=ORIENTED_EDGE('',*,*,#8604,.F.);
#11678=ORIENTED_EDGE('',*,*,#8590,.F.);
#11679=ORIENTED_EDGE('',*,*,#8631,.T.);
#11680=ORIENTED_EDGE('',*,*,#8570,.F.);
#11681=ORIENTED_EDGE('',*,*,#8574,.F.);
#11682=ORIENTED_EDGE('',*,*,#8568,.F.);
#11683=ORIENTED_EDGE('',*,*,#8632,.T.);
#11684=ORIENTED_EDGE('',*,*,#8547,.F.);
#11685=ORIENTED_EDGE('',*,*,#8551,.F.);
#11686=ORIENTED_EDGE('',*,*,#8545,.F.);
#11687=ORIENTED_EDGE('',*,*,#8633,.T.);
#11688=ORIENTED_EDGE('',*,*,#8524,.F.);
#11689=ORIENTED_EDGE('',*,*,#8528,.F.);
#11690=ORIENTED_EDGE('',*,*,#8522,.F.);
#11691=ORIENTED_EDGE('',*,*,#8634,.T.);
#11692=ORIENTED_EDGE('',*,*,#8501,.F.);
#11693=ORIENTED_EDGE('',*,*,#8505,.F.);
#11694=ORIENTED_EDGE('',*,*,#8499,.F.);
#11695=ORIENTED_EDGE('',*,*,#8635,.T.);
#11696=ORIENTED_EDGE('',*,*,#8636,.F.);
#11697=ORIENTED_EDGE('',*,*,#8637,.F.);
#11698=ORIENTED_EDGE('',*,*,#8638,.F.);
#11699=ORIENTED_EDGE('',*,*,#8639,.T.);
#11700=ORIENTED_EDGE('',*,*,#8640,.F.);
#11701=ORIENTED_EDGE('',*,*,#8641,.F.);
#11702=ORIENTED_EDGE('',*,*,#8642,.F.);
#11703=ORIENTED_EDGE('',*,*,#8643,.T.);
#11704=ORIENTED_EDGE('',*,*,#8644,.F.);
#11705=ORIENTED_EDGE('',*,*,#8645,.F.);
#11706=ORIENTED_EDGE('',*,*,#8646,.F.);
#11707=ORIENTED_EDGE('',*,*,#8647,.T.);
#11708=ORIENTED_EDGE('',*,*,#8648,.F.);
#11709=ORIENTED_EDGE('',*,*,#8649,.F.);
#11710=ORIENTED_EDGE('',*,*,#8650,.F.);
#11711=ORIENTED_EDGE('',*,*,#8651,.T.);
#11712=ORIENTED_EDGE('',*,*,#8652,.F.);
#11713=ORIENTED_EDGE('',*,*,#8653,.F.);
#11714=ORIENTED_EDGE('',*,*,#8616,.F.);
#11715=ORIENTED_EDGE('',*,*,#8654,.T.);
#11716=ORIENTED_EDGE('',*,*,#8612,.T.);
#11717=ORIENTED_EDGE('',*,*,#8630,.T.);
#11718=ORIENTED_EDGE('',*,*,#8655,.T.);
#11719=ORIENTED_EDGE('',*,*,#8628,.T.);
#11720=ORIENTED_EDGE('',*,*,#8656,.T.);
#11721=ORIENTED_EDGE('',*,*,#8657,.T.);
#11722=ORIENTED_EDGE('',*,*,#8658,.T.);
#11723=ORIENTED_EDGE('',*,*,#8629,.T.);
#11724=ORIENTED_EDGE('',*,*,#8658,.F.);
#11725=ORIENTED_EDGE('',*,*,#8659,.T.);
#11726=ORIENTED_EDGE('',*,*,#8660,.T.);
#11727=ORIENTED_EDGE('',*,*,#8661,.T.);
#11728=ORIENTED_EDGE('',*,*,#8655,.F.);
#11729=ORIENTED_EDGE('',*,*,#8654,.F.);
#11730=ORIENTED_EDGE('',*,*,#8661,.F.);
#11731=ORIENTED_EDGE('',*,*,#8662,.T.);
#11732=ORIENTED_EDGE('',*,*,#8663,.F.);
#11733=ORIENTED_EDGE('',*,*,#8664,.F.);
#11734=ORIENTED_EDGE('',*,*,#8665,.F.);
#11735=ORIENTED_EDGE('',*,*,#8613,.F.);
#11736=ORIENTED_EDGE('',*,*,#8660,.F.);
#11737=ORIENTED_EDGE('',*,*,#8666,.F.);
#11738=ORIENTED_EDGE('',*,*,#8667,.F.);
#11739=ORIENTED_EDGE('',*,*,#8662,.F.);
#11740=ORIENTED_EDGE('',*,*,#8657,.F.);
#11741=ORIENTED_EDGE('',*,*,#8668,.F.);
#11742=ORIENTED_EDGE('',*,*,#8669,.F.);
#11743=ORIENTED_EDGE('',*,*,#8670,.F.);
#11744=ORIENTED_EDGE('',*,*,#8671,.T.);
#11745=ORIENTED_EDGE('',*,*,#8666,.T.);
#11746=ORIENTED_EDGE('',*,*,#8659,.F.);
#11747=ORIENTED_EDGE('',*,*,#8672,.T.);
#11748=ORIENTED_EDGE('',*,*,#8673,.T.);
#11749=ORIENTED_EDGE('',*,*,#8626,.T.);
#11750=ORIENTED_EDGE('',*,*,#8674,.T.);
#11751=ORIENTED_EDGE('',*,*,#8624,.T.);
#11752=ORIENTED_EDGE('',*,*,#8675,.T.);
#11753=ORIENTED_EDGE('',*,*,#8676,.T.);
#11754=ORIENTED_EDGE('',*,*,#8677,.T.);
#11755=ORIENTED_EDGE('',*,*,#8625,.T.);
#11756=ORIENTED_EDGE('',*,*,#8677,.F.);
#11757=ORIENTED_EDGE('',*,*,#8678,.T.);
#11758=ORIENTED_EDGE('',*,*,#8679,.T.);
#11759=ORIENTED_EDGE('',*,*,#8680,.T.);
#11760=ORIENTED_EDGE('',*,*,#8674,.F.);
#11761=ORIENTED_EDGE('',*,*,#8672,.F.);
#11762=ORIENTED_EDGE('',*,*,#8680,.F.);
#11763=ORIENTED_EDGE('',*,*,#8681,.T.);
#11764=ORIENTED_EDGE('',*,*,#8682,.F.);
#11765=ORIENTED_EDGE('',*,*,#8683,.F.);
#11766=ORIENTED_EDGE('',*,*,#8684,.F.);
#11767=ORIENTED_EDGE('',*,*,#8685,.F.);
#11768=ORIENTED_EDGE('',*,*,#8679,.F.);
#11769=ORIENTED_EDGE('',*,*,#8686,.F.);
#11770=ORIENTED_EDGE('',*,*,#8687,.F.);
#11771=ORIENTED_EDGE('',*,*,#8681,.F.);
#11772=ORIENTED_EDGE('',*,*,#8676,.F.);
#11773=ORIENTED_EDGE('',*,*,#8688,.F.);
#11774=ORIENTED_EDGE('',*,*,#8689,.F.);
#11775=ORIENTED_EDGE('',*,*,#8690,.F.);
#11776=ORIENTED_EDGE('',*,*,#8691,.T.);
#11777=ORIENTED_EDGE('',*,*,#8686,.T.);
#11778=ORIENTED_EDGE('',*,*,#8678,.F.);
#11779=ORIENTED_EDGE('',*,*,#8692,.T.);
#11780=ORIENTED_EDGE('',*,*,#8693,.T.);
#11781=ORIENTED_EDGE('',*,*,#8694,.T.);
#11782=ORIENTED_EDGE('',*,*,#8695,.T.);
#11783=ORIENTED_EDGE('',*,*,#8693,.F.);
#11784=ORIENTED_EDGE('',*,*,#8696,.T.);
#11785=ORIENTED_EDGE('',*,*,#8697,.T.);
#11786=ORIENTED_EDGE('',*,*,#8698,.F.);
#11787=ORIENTED_EDGE('',*,*,#8699,.T.);
#11788=ORIENTED_EDGE('',*,*,#8700,.T.);
#11789=ORIENTED_EDGE('',*,*,#8701,.T.);
#11790=ORIENTED_EDGE('',*,*,#8702,.T.);
#11791=ORIENTED_EDGE('',*,*,#8700,.F.);
#11792=ORIENTED_EDGE('',*,*,#8703,.T.);
#11793=ORIENTED_EDGE('',*,*,#8704,.T.);
#11794=ORIENTED_EDGE('',*,*,#8705,.F.);
#11795=ORIENTED_EDGE('',*,*,#8706,.T.);
#11796=ORIENTED_EDGE('',*,*,#8707,.T.);
#11797=ORIENTED_EDGE('',*,*,#8708,.T.);
#11798=ORIENTED_EDGE('',*,*,#8709,.T.);
#11799=ORIENTED_EDGE('',*,*,#8707,.F.);
#11800=ORIENTED_EDGE('',*,*,#8710,.T.);
#11801=ORIENTED_EDGE('',*,*,#8711,.T.);
#11802=ORIENTED_EDGE('',*,*,#8712,.F.);
#11803=ORIENTED_EDGE('',*,*,#8713,.T.);
#11804=ORIENTED_EDGE('',*,*,#8714,.T.);
#11805=ORIENTED_EDGE('',*,*,#8715,.T.);
#11806=ORIENTED_EDGE('',*,*,#8716,.T.);
#11807=ORIENTED_EDGE('',*,*,#8714,.F.);
#11808=ORIENTED_EDGE('',*,*,#8717,.T.);
#11809=ORIENTED_EDGE('',*,*,#8718,.T.);
#11810=ORIENTED_EDGE('',*,*,#8719,.F.);
#11811=ORIENTED_EDGE('',*,*,#8720,.T.);
#11812=ORIENTED_EDGE('',*,*,#8721,.T.);
#11813=ORIENTED_EDGE('',*,*,#8722,.T.);
#11814=ORIENTED_EDGE('',*,*,#8723,.T.);
#11815=ORIENTED_EDGE('',*,*,#8721,.F.);
#11816=ORIENTED_EDGE('',*,*,#8724,.T.);
#11817=ORIENTED_EDGE('',*,*,#8725,.T.);
#11818=ORIENTED_EDGE('',*,*,#8726,.F.);
#11819=ORIENTED_EDGE('',*,*,#8683,.T.);
#11820=ORIENTED_EDGE('',*,*,#8727,.T.);
#11821=ORIENTED_EDGE('',*,*,#8690,.T.);
#11822=ORIENTED_EDGE('',*,*,#8728,.T.);
#11823=ORIENTED_EDGE('',*,*,#8727,.F.);
#11824=ORIENTED_EDGE('',*,*,#8682,.T.);
#11825=ORIENTED_EDGE('',*,*,#8687,.T.);
#11826=ORIENTED_EDGE('',*,*,#8691,.F.);
#11827=ORIENTED_EDGE('',*,*,#8664,.T.);
#11828=ORIENTED_EDGE('',*,*,#8729,.T.);
#11829=ORIENTED_EDGE('',*,*,#8670,.T.);
#11830=ORIENTED_EDGE('',*,*,#8730,.T.);
#11831=ORIENTED_EDGE('',*,*,#8729,.F.);
#11832=ORIENTED_EDGE('',*,*,#8663,.T.);
#11833=ORIENTED_EDGE('',*,*,#8667,.T.);
#11834=ORIENTED_EDGE('',*,*,#8671,.F.);
#11835=ORIENTED_EDGE('',*,*,#8596,.T.);
#11836=ORIENTED_EDGE('',*,*,#8731,.T.);
#11837=ORIENTED_EDGE('',*,*,#8608,.T.);
#11838=ORIENTED_EDGE('',*,*,#8732,.T.);
#11839=ORIENTED_EDGE('',*,*,#8731,.F.);
#11840=ORIENTED_EDGE('',*,*,#8595,.T.);
#11841=ORIENTED_EDGE('',*,*,#8733,.T.);
#11842=ORIENTED_EDGE('',*,*,#8609,.F.);
#11843=ORIENTED_EDGE('',*,*,#8580,.T.);
#11844=ORIENTED_EDGE('',*,*,#8734,.T.);
#11845=ORIENTED_EDGE('',*,*,#8587,.T.);
#11846=ORIENTED_EDGE('',*,*,#8735,.T.);
#11847=ORIENTED_EDGE('',*,*,#8734,.F.);
#11848=ORIENTED_EDGE('',*,*,#8579,.T.);
#11849=ORIENTED_EDGE('',*,*,#8584,.T.);
#11850=ORIENTED_EDGE('',*,*,#8588,.F.);
#11851=ORIENTED_EDGE('',*,*,#8557,.T.);
#11852=ORIENTED_EDGE('',*,*,#8736,.T.);
#11853=ORIENTED_EDGE('',*,*,#8564,.T.);
#11854=ORIENTED_EDGE('',*,*,#8737,.T.);
#11855=ORIENTED_EDGE('',*,*,#8736,.F.);
#11856=ORIENTED_EDGE('',*,*,#8556,.T.);
#11857=ORIENTED_EDGE('',*,*,#8561,.T.);
#11858=ORIENTED_EDGE('',*,*,#8565,.F.);
#11859=ORIENTED_EDGE('',*,*,#8534,.T.);
#11860=ORIENTED_EDGE('',*,*,#8738,.T.);
#11861=ORIENTED_EDGE('',*,*,#8541,.T.);
#11862=ORIENTED_EDGE('',*,*,#8739,.T.);
#11863=ORIENTED_EDGE('',*,*,#8738,.F.);
#11864=ORIENTED_EDGE('',*,*,#8533,.T.);
#11865=ORIENTED_EDGE('',*,*,#8538,.T.);
#11866=ORIENTED_EDGE('',*,*,#8542,.F.);
#11867=ORIENTED_EDGE('',*,*,#8511,.T.);
#11868=ORIENTED_EDGE('',*,*,#8740,.T.);
#11869=ORIENTED_EDGE('',*,*,#8518,.T.);
#11870=ORIENTED_EDGE('',*,*,#8741,.T.);
#11871=ORIENTED_EDGE('',*,*,#8740,.F.);
#11872=ORIENTED_EDGE('',*,*,#8510,.T.);
#11873=ORIENTED_EDGE('',*,*,#8515,.T.);
#11874=ORIENTED_EDGE('',*,*,#8519,.F.);
#11875=ORIENTED_EDGE('',*,*,#8742,.T.);
#11876=ORIENTED_EDGE('',*,*,#8743,.T.);
#11877=ORIENTED_EDGE('',*,*,#8622,.T.);
#11878=ORIENTED_EDGE('',*,*,#8744,.T.);
#11879=ORIENTED_EDGE('',*,*,#8620,.T.);
#11880=ORIENTED_EDGE('',*,*,#8745,.T.);
#11881=ORIENTED_EDGE('',*,*,#8746,.T.);
#11882=ORIENTED_EDGE('',*,*,#8747,.T.);
#11883=ORIENTED_EDGE('',*,*,#8621,.T.);
#11884=ORIENTED_EDGE('',*,*,#8747,.F.);
#11885=ORIENTED_EDGE('',*,*,#8748,.T.);
#11886=ORIENTED_EDGE('',*,*,#8749,.T.);
#11887=ORIENTED_EDGE('',*,*,#8750,.T.);
#11888=ORIENTED_EDGE('',*,*,#8744,.F.);
#11889=ORIENTED_EDGE('',*,*,#8742,.F.);
#11890=ORIENTED_EDGE('',*,*,#8750,.F.);
#11891=ORIENTED_EDGE('',*,*,#8751,.T.);
#11892=ORIENTED_EDGE('',*,*,#8724,.F.);
#11893=ORIENTED_EDGE('',*,*,#8720,.F.);
#11894=ORIENTED_EDGE('',*,*,#8752,.F.);
#11895=ORIENTED_EDGE('',*,*,#8753,.F.);
#11896=ORIENTED_EDGE('',*,*,#8749,.F.);
#11897=ORIENTED_EDGE('',*,*,#8754,.F.);
#11898=ORIENTED_EDGE('',*,*,#8725,.F.);
#11899=ORIENTED_EDGE('',*,*,#8751,.F.);
#11900=ORIENTED_EDGE('',*,*,#8746,.F.);
#11901=ORIENTED_EDGE('',*,*,#8755,.F.);
#11902=ORIENTED_EDGE('',*,*,#8756,.F.);
#11903=ORIENTED_EDGE('',*,*,#8722,.F.);
#11904=ORIENTED_EDGE('',*,*,#8726,.T.);
#11905=ORIENTED_EDGE('',*,*,#8754,.T.);
#11906=ORIENTED_EDGE('',*,*,#8748,.F.);
#11907=ORIENTED_EDGE('',*,*,#8757,.T.);
#11908=ORIENTED_EDGE('',*,*,#8758,.T.);
#11909=ORIENTED_EDGE('',*,*,#8618,.T.);
#11910=ORIENTED_EDGE('',*,*,#8759,.T.);
#11911=ORIENTED_EDGE('',*,*,#8652,.T.);
#11912=ORIENTED_EDGE('',*,*,#8760,.T.);
#11913=ORIENTED_EDGE('',*,*,#8761,.T.);
#11914=ORIENTED_EDGE('',*,*,#8762,.T.);
#11915=ORIENTED_EDGE('',*,*,#8617,.T.);
#11916=ORIENTED_EDGE('',*,*,#8653,.T.);
#11917=ORIENTED_EDGE('',*,*,#8762,.F.);
#11918=ORIENTED_EDGE('',*,*,#8763,.T.);
#11919=ORIENTED_EDGE('',*,*,#8764,.T.);
#11920=ORIENTED_EDGE('',*,*,#8765,.T.);
#11921=ORIENTED_EDGE('',*,*,#8759,.F.);
#11922=ORIENTED_EDGE('',*,*,#8757,.F.);
#11923=ORIENTED_EDGE('',*,*,#8765,.F.);
#11924=ORIENTED_EDGE('',*,*,#8766,.T.);
#11925=ORIENTED_EDGE('',*,*,#8717,.F.);
#11926=ORIENTED_EDGE('',*,*,#8713,.F.);
#11927=ORIENTED_EDGE('',*,*,#8767,.F.);
#11928=ORIENTED_EDGE('',*,*,#8768,.F.);
#11929=ORIENTED_EDGE('',*,*,#8764,.F.);
#11930=ORIENTED_EDGE('',*,*,#8769,.F.);
#11931=ORIENTED_EDGE('',*,*,#8718,.F.);
#11932=ORIENTED_EDGE('',*,*,#8766,.F.);
#11933=ORIENTED_EDGE('',*,*,#8761,.F.);
#11934=ORIENTED_EDGE('',*,*,#8770,.F.);
#11935=ORIENTED_EDGE('',*,*,#8771,.F.);
#11936=ORIENTED_EDGE('',*,*,#8715,.F.);
#11937=ORIENTED_EDGE('',*,*,#8719,.T.);
#11938=ORIENTED_EDGE('',*,*,#8769,.T.);
#11939=ORIENTED_EDGE('',*,*,#8763,.F.);
#11940=ORIENTED_EDGE('',*,*,#8772,.T.);
#11941=ORIENTED_EDGE('',*,*,#8773,.T.);
#11942=ORIENTED_EDGE('',*,*,#8650,.T.);
#11943=ORIENTED_EDGE('',*,*,#8774,.T.);
#11944=ORIENTED_EDGE('',*,*,#8648,.T.);
#11945=ORIENTED_EDGE('',*,*,#8775,.T.);
#11946=ORIENTED_EDGE('',*,*,#8776,.T.);
#11947=ORIENTED_EDGE('',*,*,#8777,.T.);
#11948=ORIENTED_EDGE('',*,*,#8649,.T.);
#11949=ORIENTED_EDGE('',*,*,#8777,.F.);
#11950=ORIENTED_EDGE('',*,*,#8778,.T.);
#11951=ORIENTED_EDGE('',*,*,#8779,.T.);
#11952=ORIENTED_EDGE('',*,*,#8780,.T.);
#11953=ORIENTED_EDGE('',*,*,#8774,.F.);
#11954=ORIENTED_EDGE('',*,*,#8772,.F.);
#11955=ORIENTED_EDGE('',*,*,#8780,.F.);
#11956=ORIENTED_EDGE('',*,*,#8781,.T.);
#11957=ORIENTED_EDGE('',*,*,#8710,.F.);
#11958=ORIENTED_EDGE('',*,*,#8706,.F.);
#11959=ORIENTED_EDGE('',*,*,#8782,.F.);
#11960=ORIENTED_EDGE('',*,*,#8783,.F.);
#11961=ORIENTED_EDGE('',*,*,#8779,.F.);
#11962=ORIENTED_EDGE('',*,*,#8784,.F.);
#11963=ORIENTED_EDGE('',*,*,#8711,.F.);
#11964=ORIENTED_EDGE('',*,*,#8781,.F.);
#11965=ORIENTED_EDGE('',*,*,#8776,.F.);
#11966=ORIENTED_EDGE('',*,*,#8785,.F.);
#11967=ORIENTED_EDGE('',*,*,#8786,.F.);
#11968=ORIENTED_EDGE('',*,*,#8708,.F.);
#11969=ORIENTED_EDGE('',*,*,#8712,.T.);
#11970=ORIENTED_EDGE('',*,*,#8784,.T.);
#11971=ORIENTED_EDGE('',*,*,#8778,.F.);
#11972=ORIENTED_EDGE('',*,*,#8787,.T.);
#11973=ORIENTED_EDGE('',*,*,#8788,.T.);
#11974=ORIENTED_EDGE('',*,*,#8646,.T.);
#11975=ORIENTED_EDGE('',*,*,#8789,.T.);
#11976=ORIENTED_EDGE('',*,*,#8644,.T.);
#11977=ORIENTED_EDGE('',*,*,#8790,.T.);
#11978=ORIENTED_EDGE('',*,*,#8791,.T.);
#11979=ORIENTED_EDGE('',*,*,#8792,.T.);
#11980=ORIENTED_EDGE('',*,*,#8645,.T.);
#11981=ORIENTED_EDGE('',*,*,#8792,.F.);
#11982=ORIENTED_EDGE('',*,*,#8793,.T.);
#11983=ORIENTED_EDGE('',*,*,#8794,.T.);
#11984=ORIENTED_EDGE('',*,*,#8795,.T.);
#11985=ORIENTED_EDGE('',*,*,#8789,.F.);
#11986=ORIENTED_EDGE('',*,*,#8787,.F.);
#11987=ORIENTED_EDGE('',*,*,#8795,.F.);
#11988=ORIENTED_EDGE('',*,*,#8796,.T.);
#11989=ORIENTED_EDGE('',*,*,#8703,.F.);
#11990=ORIENTED_EDGE('',*,*,#8699,.F.);
#11991=ORIENTED_EDGE('',*,*,#8797,.F.);
#11992=ORIENTED_EDGE('',*,*,#8798,.F.);
#11993=ORIENTED_EDGE('',*,*,#8794,.F.);
#11994=ORIENTED_EDGE('',*,*,#8799,.F.);
#11995=ORIENTED_EDGE('',*,*,#8704,.F.);
#11996=ORIENTED_EDGE('',*,*,#8796,.F.);
#11997=ORIENTED_EDGE('',*,*,#8791,.F.);
#11998=ORIENTED_EDGE('',*,*,#8800,.F.);
#11999=ORIENTED_EDGE('',*,*,#8801,.F.);
#12000=ORIENTED_EDGE('',*,*,#8701,.F.);
#12001=ORIENTED_EDGE('',*,*,#8705,.T.);
#12002=ORIENTED_EDGE('',*,*,#8799,.T.);
#12003=ORIENTED_EDGE('',*,*,#8793,.F.);
#12004=ORIENTED_EDGE('',*,*,#8802,.T.);
#12005=ORIENTED_EDGE('',*,*,#8803,.T.);
#12006=ORIENTED_EDGE('',*,*,#8642,.T.);
#12007=ORIENTED_EDGE('',*,*,#8804,.T.);
#12008=ORIENTED_EDGE('',*,*,#8640,.T.);
#12009=ORIENTED_EDGE('',*,*,#8805,.T.);
#12010=ORIENTED_EDGE('',*,*,#8806,.T.);
#12011=ORIENTED_EDGE('',*,*,#8807,.T.);
#12012=ORIENTED_EDGE('',*,*,#8641,.T.);
#12013=ORIENTED_EDGE('',*,*,#8807,.F.);
#12014=ORIENTED_EDGE('',*,*,#8808,.T.);
#12015=ORIENTED_EDGE('',*,*,#8809,.T.);
#12016=ORIENTED_EDGE('',*,*,#8810,.T.);
#12017=ORIENTED_EDGE('',*,*,#8804,.F.);
#12018=ORIENTED_EDGE('',*,*,#8809,.F.);
#12019=ORIENTED_EDGE('',*,*,#8811,.F.);
#12020=ORIENTED_EDGE('',*,*,#8697,.F.);
#12021=ORIENTED_EDGE('',*,*,#8812,.F.);
#12022=ORIENTED_EDGE('',*,*,#8806,.F.);
#12023=ORIENTED_EDGE('',*,*,#8813,.F.);
#12024=ORIENTED_EDGE('',*,*,#8814,.F.);
#12025=ORIENTED_EDGE('',*,*,#8694,.F.);
#12026=ORIENTED_EDGE('',*,*,#8698,.T.);
#12027=ORIENTED_EDGE('',*,*,#8811,.T.);
#12028=ORIENTED_EDGE('',*,*,#8808,.F.);
#12029=ORIENTED_EDGE('',*,*,#8805,.F.);
#12030=ORIENTED_EDGE('',*,*,#8639,.F.);
#12031=ORIENTED_EDGE('',*,*,#8815,.F.);
#12032=ORIENTED_EDGE('',*,*,#8816,.T.);
#12033=ORIENTED_EDGE('',*,*,#8817,.T.);
#12034=ORIENTED_EDGE('',*,*,#8813,.T.);
#12035=ORIENTED_EDGE('',*,*,#8818,.T.);
#12036=ORIENTED_EDGE('',*,*,#8819,.T.);
#12037=ORIENTED_EDGE('',*,*,#8820,.T.);
#12038=ORIENTED_EDGE('',*,*,#8821,.T.);
#12039=ORIENTED_EDGE('',*,*,#8819,.F.);
#12040=ORIENTED_EDGE('',*,*,#8822,.T.);
#12041=ORIENTED_EDGE('',*,*,#8823,.T.);
#12042=ORIENTED_EDGE('',*,*,#8824,.F.);
#12043=ORIENTED_EDGE('',*,*,#8825,.T.);
#12044=ORIENTED_EDGE('',*,*,#8815,.T.);
#12045=ORIENTED_EDGE('',*,*,#8638,.T.);
#12046=ORIENTED_EDGE('',*,*,#8826,.T.);
#12047=ORIENTED_EDGE('',*,*,#8636,.T.);
#12048=ORIENTED_EDGE('',*,*,#8827,.T.);
#12049=ORIENTED_EDGE('',*,*,#8828,.T.);
#12050=ORIENTED_EDGE('',*,*,#8829,.T.);
#12051=ORIENTED_EDGE('',*,*,#8637,.T.);
#12052=ORIENTED_EDGE('',*,*,#8829,.F.);
#12053=ORIENTED_EDGE('',*,*,#8830,.T.);
#12054=ORIENTED_EDGE('',*,*,#8831,.T.);
#12055=ORIENTED_EDGE('',*,*,#8832,.T.);
#12056=ORIENTED_EDGE('',*,*,#8826,.F.);
#12057=ORIENTED_EDGE('',*,*,#8831,.F.);
#12058=ORIENTED_EDGE('',*,*,#8833,.F.);
#12059=ORIENTED_EDGE('',*,*,#8823,.F.);
#12060=ORIENTED_EDGE('',*,*,#8834,.F.);
#12061=ORIENTED_EDGE('',*,*,#8828,.F.);
#12062=ORIENTED_EDGE('',*,*,#8835,.F.);
#12063=ORIENTED_EDGE('',*,*,#8836,.F.);
#12064=ORIENTED_EDGE('',*,*,#8820,.F.);
#12065=ORIENTED_EDGE('',*,*,#8824,.T.);
#12066=ORIENTED_EDGE('',*,*,#8833,.T.);
#12067=ORIENTED_EDGE('',*,*,#8830,.F.);
#12068=ORIENTED_EDGE('',*,*,#8498,.F.);
#12069=ORIENTED_EDGE('',*,*,#8513,.T.);
#12070=ORIENTED_EDGE('',*,*,#8837,.T.);
#12071=ORIENTED_EDGE('',*,*,#8835,.T.);
#12072=ORIENTED_EDGE('',*,*,#8827,.F.);
#12073=ORIENTED_EDGE('',*,*,#8635,.F.);
#12074=ORIENTED_EDGE('',*,*,#8838,.T.);
#12075=ORIENTED_EDGE('',*,*,#8839,.T.);
#12076=ORIENTED_EDGE('',*,*,#8840,.T.);
#12077=ORIENTED_EDGE('',*,*,#8839,.F.);
#12078=ORIENTED_EDGE('',*,*,#8840,.F.);
#12079=ORIENTED_EDGE('',*,*,#8841,.T.);
#12080=ORIENTED_EDGE('',*,*,#8842,.T.);
#12081=ORIENTED_EDGE('',*,*,#8841,.F.);
#12082=ORIENTED_EDGE('',*,*,#8814,.T.);
#12083=ORIENTED_EDGE('',*,*,#8817,.F.);
#12084=ORIENTED_EDGE('',*,*,#8843,.T.);
#12085=ORIENTED_EDGE('',*,*,#8821,.F.);
#12086=ORIENTED_EDGE('',*,*,#8836,.T.);
#12087=ORIENTED_EDGE('',*,*,#8837,.F.);
#12088=ORIENTED_EDGE('',*,*,#8512,.T.);
#12089=ORIENTED_EDGE('',*,*,#8741,.F.);
#12090=ORIENTED_EDGE('',*,*,#8517,.T.);
#12091=ORIENTED_EDGE('',*,*,#8844,.F.);
#12092=ORIENTED_EDGE('',*,*,#8535,.T.);
#12093=ORIENTED_EDGE('',*,*,#8739,.F.);
#12094=ORIENTED_EDGE('',*,*,#8540,.T.);
#12095=ORIENTED_EDGE('',*,*,#8845,.F.);
#12096=ORIENTED_EDGE('',*,*,#8558,.T.);
#12097=ORIENTED_EDGE('',*,*,#8737,.F.);
#12098=ORIENTED_EDGE('',*,*,#8563,.T.);
#12099=ORIENTED_EDGE('',*,*,#8846,.F.);
#12100=ORIENTED_EDGE('',*,*,#8581,.T.);
#12101=ORIENTED_EDGE('',*,*,#8735,.F.);
#12102=ORIENTED_EDGE('',*,*,#8586,.T.);
#12103=ORIENTED_EDGE('',*,*,#8847,.F.);
#12104=ORIENTED_EDGE('',*,*,#8597,.T.);
#12105=ORIENTED_EDGE('',*,*,#8732,.F.);
#12106=ORIENTED_EDGE('',*,*,#8607,.T.);
#12107=ORIENTED_EDGE('',*,*,#8614,.F.);
#12108=ORIENTED_EDGE('',*,*,#8665,.T.);
#12109=ORIENTED_EDGE('',*,*,#8730,.F.);
#12110=ORIENTED_EDGE('',*,*,#8669,.T.);
#12111=ORIENTED_EDGE('',*,*,#8848,.F.);
#12112=ORIENTED_EDGE('',*,*,#8684,.T.);
#12113=ORIENTED_EDGE('',*,*,#8728,.F.);
#12114=ORIENTED_EDGE('',*,*,#8689,.T.);
#12115=ORIENTED_EDGE('',*,*,#8849,.F.);
#12116=ORIENTED_EDGE('',*,*,#8752,.T.);
#12117=ORIENTED_EDGE('',*,*,#8723,.F.);
#12118=ORIENTED_EDGE('',*,*,#8756,.T.);
#12119=ORIENTED_EDGE('',*,*,#8850,.F.);
#12120=ORIENTED_EDGE('',*,*,#8767,.T.);
#12121=ORIENTED_EDGE('',*,*,#8716,.F.);
#12122=ORIENTED_EDGE('',*,*,#8771,.T.);
#12123=ORIENTED_EDGE('',*,*,#8851,.F.);
#12124=ORIENTED_EDGE('',*,*,#8782,.T.);
#12125=ORIENTED_EDGE('',*,*,#8709,.F.);
#12126=ORIENTED_EDGE('',*,*,#8786,.T.);
#12127=ORIENTED_EDGE('',*,*,#8852,.F.);
#12128=ORIENTED_EDGE('',*,*,#8797,.T.);
#12129=ORIENTED_EDGE('',*,*,#8702,.F.);
#12130=ORIENTED_EDGE('',*,*,#8801,.T.);
#12131=ORIENTED_EDGE('',*,*,#8853,.F.);
#12132=ORIENTED_EDGE('',*,*,#8854,.T.);
#12133=ORIENTED_EDGE('',*,*,#8695,.F.);
#12134=ORIENTED_EDGE('',*,*,#8838,.F.);
#12135=ORIENTED_EDGE('',*,*,#8842,.F.);
#12136=ORIENTED_EDGE('',*,*,#8855,.F.);
#12137=ORIENTED_EDGE('',*,*,#8856,.T.);
#12138=ORIENTED_EDGE('',*,*,#8857,.T.);
#12139=ORIENTED_EDGE('',*,*,#8858,.F.);
#12140=ORIENTED_EDGE('',*,*,#8859,.F.);
#12141=ORIENTED_EDGE('',*,*,#8858,.T.);
#12142=ORIENTED_EDGE('',*,*,#8860,.T.);
#12143=ORIENTED_EDGE('',*,*,#8861,.F.);
#12144=ORIENTED_EDGE('',*,*,#8862,.F.);
#12145=ORIENTED_EDGE('',*,*,#8863,.T.);
#12146=ORIENTED_EDGE('',*,*,#8864,.T.);
#12147=ORIENTED_EDGE('',*,*,#8856,.F.);
#12148=ORIENTED_EDGE('',*,*,#8865,.F.);
#12149=ORIENTED_EDGE('',*,*,#8861,.T.);
#12150=ORIENTED_EDGE('',*,*,#8866,.T.);
#12151=ORIENTED_EDGE('',*,*,#8863,.F.);
#12152=ORIENTED_EDGE('',*,*,#8857,.F.);
#12153=ORIENTED_EDGE('',*,*,#8864,.F.);
#12154=ORIENTED_EDGE('',*,*,#8866,.F.);
#12155=ORIENTED_EDGE('',*,*,#8860,.F.);
#12156=ORIENTED_EDGE('',*,*,#8825,.F.);
#12157=ORIENTED_EDGE('',*,*,#8832,.F.);
#12158=ORIENTED_EDGE('',*,*,#8834,.T.);
#12159=ORIENTED_EDGE('',*,*,#8822,.F.);
#12160=ORIENTED_EDGE('',*,*,#8818,.F.);
#12161=ORIENTED_EDGE('',*,*,#8843,.F.);
#12162=ORIENTED_EDGE('',*,*,#8816,.F.);
#12163=ORIENTED_EDGE('',*,*,#8502,.F.);
#12164=ORIENTED_EDGE('',*,*,#8634,.F.);
#12165=ORIENTED_EDGE('',*,*,#8521,.F.);
#12166=ORIENTED_EDGE('',*,*,#8536,.T.);
#12167=ORIENTED_EDGE('',*,*,#8844,.T.);
#12168=ORIENTED_EDGE('',*,*,#8516,.T.);
#12169=ORIENTED_EDGE('',*,*,#8525,.F.);
#12170=ORIENTED_EDGE('',*,*,#8633,.F.);
#12171=ORIENTED_EDGE('',*,*,#8544,.F.);
#12172=ORIENTED_EDGE('',*,*,#8559,.T.);
#12173=ORIENTED_EDGE('',*,*,#8845,.T.);
#12174=ORIENTED_EDGE('',*,*,#8539,.T.);
#12175=ORIENTED_EDGE('',*,*,#8548,.F.);
#12176=ORIENTED_EDGE('',*,*,#8632,.F.);
#12177=ORIENTED_EDGE('',*,*,#8567,.F.);
#12178=ORIENTED_EDGE('',*,*,#8582,.T.);
#12179=ORIENTED_EDGE('',*,*,#8846,.T.);
#12180=ORIENTED_EDGE('',*,*,#8562,.T.);
#12181=ORIENTED_EDGE('',*,*,#8571,.F.);
#12182=ORIENTED_EDGE('',*,*,#8631,.F.);
#12183=ORIENTED_EDGE('',*,*,#8589,.F.);
#12184=ORIENTED_EDGE('',*,*,#8598,.T.);
#12185=ORIENTED_EDGE('',*,*,#8847,.T.);
#12186=ORIENTED_EDGE('',*,*,#8585,.T.);
#12187=ORIENTED_EDGE('',*,*,#8603,.F.);
#12188=ORIENTED_EDGE('',*,*,#8610,.F.);
#12189=ORIENTED_EDGE('',*,*,#8733,.F.);
#12190=ORIENTED_EDGE('',*,*,#8594,.F.);
#12191=ORIENTED_EDGE('',*,*,#8656,.F.);
#12192=ORIENTED_EDGE('',*,*,#8627,.F.);
#12193=ORIENTED_EDGE('',*,*,#8673,.F.);
#12194=ORIENTED_EDGE('',*,*,#8685,.T.);
#12195=ORIENTED_EDGE('',*,*,#8848,.T.);
#12196=ORIENTED_EDGE('',*,*,#8668,.T.);
#12197=ORIENTED_EDGE('',*,*,#8675,.F.);
#12198=ORIENTED_EDGE('',*,*,#8623,.F.);
#12199=ORIENTED_EDGE('',*,*,#8743,.F.);
#12200=ORIENTED_EDGE('',*,*,#8753,.T.);
#12201=ORIENTED_EDGE('',*,*,#8849,.T.);
#12202=ORIENTED_EDGE('',*,*,#8688,.T.);
#12203=ORIENTED_EDGE('',*,*,#8745,.F.);
#12204=ORIENTED_EDGE('',*,*,#8619,.F.);
#12205=ORIENTED_EDGE('',*,*,#8758,.F.);
#12206=ORIENTED_EDGE('',*,*,#8768,.T.);
#12207=ORIENTED_EDGE('',*,*,#8850,.T.);
#12208=ORIENTED_EDGE('',*,*,#8755,.T.);
#12209=ORIENTED_EDGE('',*,*,#8760,.F.);
#12210=ORIENTED_EDGE('',*,*,#8651,.F.);
#12211=ORIENTED_EDGE('',*,*,#8773,.F.);
#12212=ORIENTED_EDGE('',*,*,#8783,.T.);
#12213=ORIENTED_EDGE('',*,*,#8851,.T.);
#12214=ORIENTED_EDGE('',*,*,#8770,.T.);
#12215=ORIENTED_EDGE('',*,*,#8775,.F.);
#12216=ORIENTED_EDGE('',*,*,#8647,.F.);
#12217=ORIENTED_EDGE('',*,*,#8788,.F.);
#12218=ORIENTED_EDGE('',*,*,#8798,.T.);
#12219=ORIENTED_EDGE('',*,*,#8852,.T.);
#12220=ORIENTED_EDGE('',*,*,#8785,.T.);
#12221=ORIENTED_EDGE('',*,*,#8802,.F.);
#12222=ORIENTED_EDGE('',*,*,#8810,.F.);
#12223=ORIENTED_EDGE('',*,*,#8812,.T.);
#12224=ORIENTED_EDGE('',*,*,#8696,.F.);
#12225=ORIENTED_EDGE('',*,*,#8692,.F.);
#12226=ORIENTED_EDGE('',*,*,#8854,.F.);
#12227=ORIENTED_EDGE('',*,*,#8867,.F.);
#12228=ORIENTED_EDGE('',*,*,#8790,.F.);
#12229=ORIENTED_EDGE('',*,*,#8643,.F.);
#12230=ORIENTED_EDGE('',*,*,#8803,.F.);
#12231=ORIENTED_EDGE('',*,*,#8867,.T.);
#12232=ORIENTED_EDGE('',*,*,#8853,.T.);
#12233=ORIENTED_EDGE('',*,*,#8800,.T.);
#12234=ORIENTED_EDGE('',*,*,#8868,.F.);
#12235=ORIENTED_EDGE('',*,*,#8615,.T.);
#12236=ORIENTED_EDGE('',*,*,#8869,.F.);
#12237=ORIENTED_EDGE('',*,*,#8870,.T.);
#12238=ORIENTED_EDGE('',*,*,#8868,.T.);
#12239=ORIENTED_EDGE('',*,*,#8870,.F.);
#12240=ORIENTED_EDGE('',*,*,#8869,.T.);
#12241=ORIENTED_EDGE('',*,*,#8871,.F.);
#12242=ORIENTED_EDGE('',*,*,#8872,.F.);
#12243=ORIENTED_EDGE('',*,*,#8873,.T.);
#12244=ORIENTED_EDGE('',*,*,#8871,.T.);
#12245=ORIENTED_EDGE('',*,*,#8873,.F.);
#12246=ORIENTED_EDGE('',*,*,#8872,.T.);
#12247=ORIENTED_EDGE('',*,*,#8874,.F.);
#12248=ORIENTED_EDGE('',*,*,#8875,.F.);
#12249=ORIENTED_EDGE('',*,*,#8876,.T.);
#12250=ORIENTED_EDGE('',*,*,#8874,.T.);
#12251=ORIENTED_EDGE('',*,*,#8876,.F.);
#12252=ORIENTED_EDGE('',*,*,#8865,.T.);
#12253=ORIENTED_EDGE('',*,*,#8862,.T.);
#12254=ORIENTED_EDGE('',*,*,#8855,.T.);
#12255=ORIENTED_EDGE('',*,*,#8859,.T.);
#12256=ORIENTED_EDGE('',*,*,#8877,.F.);
#12257=ORIENTED_EDGE('',*,*,#8878,.T.);
#12258=ORIENTED_EDGE('',*,*,#8875,.T.);
#12259=ORIENTED_EDGE('',*,*,#8878,.F.);
#12260=ORIENTED_EDGE('',*,*,#8877,.T.);
#12261=ORIENTED_EDGE('',*,*,#8879,.T.);
#12262=ORIENTED_EDGE('',*,*,#8880,.T.);
#12263=ORIENTED_EDGE('',*,*,#8881,.T.);
#12264=ORIENTED_EDGE('',*,*,#8882,.T.);
#12265=ORIENTED_EDGE('',*,*,#8883,.T.);
#12266=ORIENTED_EDGE('',*,*,#8884,.T.);
#12267=ORIENTED_EDGE('',*,*,#8880,.F.);
#12268=ORIENTED_EDGE('',*,*,#8885,.F.);
#12269=ORIENTED_EDGE('',*,*,#8886,.F.);
#12270=ORIENTED_EDGE('',*,*,#8887,.F.);
#12271=ORIENTED_EDGE('',*,*,#8879,.F.);
#12272=ORIENTED_EDGE('',*,*,#8888,.F.);
#12273=ORIENTED_EDGE('',*,*,#8889,.T.);
#12274=ORIENTED_EDGE('',*,*,#8890,.F.);
#12275=ORIENTED_EDGE('',*,*,#8891,.F.);
#12276=ORIENTED_EDGE('',*,*,#8885,.T.);
#12277=ORIENTED_EDGE('',*,*,#8884,.F.);
#12278=ORIENTED_EDGE('',*,*,#8892,.T.);
#12279=ORIENTED_EDGE('',*,*,#8893,.F.);
#12280=ORIENTED_EDGE('',*,*,#8894,.T.);
#12281=ORIENTED_EDGE('',*,*,#8895,.T.);
#12282=ORIENTED_EDGE('',*,*,#8888,.T.);
#12283=ORIENTED_EDGE('',*,*,#8896,.T.);
#12284=ORIENTED_EDGE('',*,*,#8897,.T.);
#12285=ORIENTED_EDGE('',*,*,#8898,.T.);
#12286=ORIENTED_EDGE('',*,*,#8893,.T.);
#12287=ORIENTED_EDGE('',*,*,#8899,.T.);
#12288=ORIENTED_EDGE('',*,*,#8900,.T.);
#12289=ORIENTED_EDGE('',*,*,#8897,.F.);
#12290=ORIENTED_EDGE('',*,*,#8901,.F.);
#12291=ORIENTED_EDGE('',*,*,#8902,.F.);
#12292=ORIENTED_EDGE('',*,*,#8903,.F.);
#12293=ORIENTED_EDGE('',*,*,#8896,.F.);
#12294=ORIENTED_EDGE('',*,*,#8904,.F.);
#12295=ORIENTED_EDGE('',*,*,#8905,.T.);
#12296=ORIENTED_EDGE('',*,*,#8906,.F.);
#12297=ORIENTED_EDGE('',*,*,#8907,.F.);
#12298=ORIENTED_EDGE('',*,*,#8901,.T.);
#12299=ORIENTED_EDGE('',*,*,#8882,.F.);
#12300=ORIENTED_EDGE('',*,*,#8908,.T.);
#12301=ORIENTED_EDGE('',*,*,#8909,.T.);
#12302=ORIENTED_EDGE('',*,*,#8904,.T.);
#12303=ORIENTED_EDGE('',*,*,#8900,.F.);
#12304=ORIENTED_EDGE('',*,*,#8910,.T.);
#12305=ORIENTED_EDGE('',*,*,#8895,.F.);
#12306=ORIENTED_EDGE('',*,*,#8911,.F.);
#12307=ORIENTED_EDGE('',*,*,#8912,.F.);
#12308=ORIENTED_EDGE('',*,*,#8889,.F.);
#12309=ORIENTED_EDGE('',*,*,#8913,.T.);
#12310=ORIENTED_EDGE('',*,*,#8914,.T.);
#12311=ORIENTED_EDGE('',*,*,#8915,.T.);
#12312=ORIENTED_EDGE('',*,*,#8916,.T.);
#12313=ORIENTED_EDGE('',*,*,#8902,.T.);
#12314=ORIENTED_EDGE('',*,*,#8907,.T.);
#12315=ORIENTED_EDGE('',*,*,#8915,.F.);
#12316=ORIENTED_EDGE('',*,*,#8917,.T.);
#12317=ORIENTED_EDGE('',*,*,#8918,.T.);
#12318=ORIENTED_EDGE('',*,*,#8890,.T.);
#12319=ORIENTED_EDGE('',*,*,#8912,.T.);
#12320=ORIENTED_EDGE('',*,*,#8919,.T.);
#12321=ORIENTED_EDGE('',*,*,#8914,.F.);
#12322=ORIENTED_EDGE('',*,*,#8920,.F.);
#12323=ORIENTED_EDGE('',*,*,#8921,.F.);
#12324=ORIENTED_EDGE('',*,*,#8917,.F.);
#12325=ORIENTED_EDGE('',*,*,#8913,.F.);
#12326=ORIENTED_EDGE('',*,*,#8906,.T.);
#12327=ORIENTED_EDGE('',*,*,#8922,.T.);
#12328=ORIENTED_EDGE('',*,*,#8923,.T.);
#12329=ORIENTED_EDGE('',*,*,#8924,.F.);
#12330=ORIENTED_EDGE('',*,*,#8920,.T.);
#12331=ORIENTED_EDGE('',*,*,#8918,.F.);
#12332=ORIENTED_EDGE('',*,*,#8921,.T.);
#12333=ORIENTED_EDGE('',*,*,#8924,.T.);
#12334=ORIENTED_EDGE('',*,*,#8925,.T.);
#12335=ORIENTED_EDGE('',*,*,#8886,.T.);
#12336=ORIENTED_EDGE('',*,*,#8891,.T.);
#12337=ORIENTED_EDGE('',*,*,#8881,.F.);
#12338=ORIENTED_EDGE('',*,*,#8887,.T.);
#12339=ORIENTED_EDGE('',*,*,#8925,.F.);
#12340=ORIENTED_EDGE('',*,*,#8923,.F.);
#12341=ORIENTED_EDGE('',*,*,#8926,.T.);
#12342=ORIENTED_EDGE('',*,*,#8908,.F.);
#12343=ORIENTED_EDGE('',*,*,#8909,.F.);
#12344=ORIENTED_EDGE('',*,*,#8926,.F.);
#12345=ORIENTED_EDGE('',*,*,#8922,.F.);
#12346=ORIENTED_EDGE('',*,*,#8905,.F.);
#12347=ORIENTED_EDGE('',*,*,#8898,.F.);
#12348=ORIENTED_EDGE('',*,*,#8903,.T.);
#12349=ORIENTED_EDGE('',*,*,#8916,.F.);
#12350=ORIENTED_EDGE('',*,*,#8919,.F.);
#12351=ORIENTED_EDGE('',*,*,#8911,.T.);
#12352=ORIENTED_EDGE('',*,*,#8894,.F.);
#12353=ORIENTED_EDGE('',*,*,#8883,.F.);
#12354=ORIENTED_EDGE('',*,*,#8910,.F.);
#12355=ORIENTED_EDGE('',*,*,#8899,.F.);
#12356=ORIENTED_EDGE('',*,*,#8892,.F.);
#12357=ORIENTED_EDGE('',*,*,#8927,.F.);
#12358=ORIENTED_EDGE('',*,*,#8928,.T.);
#12359=ORIENTED_EDGE('',*,*,#8929,.T.);
#12360=ORIENTED_EDGE('',*,*,#8928,.F.);
#12361=ORIENTED_EDGE('',*,*,#8930,.F.);
#12362=ORIENTED_EDGE('',*,*,#8927,.T.);
#12363=ORIENTED_EDGE('',*,*,#8930,.T.);
#12364=ORIENTED_EDGE('',*,*,#8931,.T.);
#12365=ORIENTED_EDGE('',*,*,#8932,.F.);
#12366=ORIENTED_EDGE('',*,*,#8931,.F.);
#12367=ORIENTED_EDGE('',*,*,#8933,.F.);
#12368=ORIENTED_EDGE('',*,*,#8932,.T.);
#12369=ORIENTED_EDGE('',*,*,#8934,.F.);
#12370=ORIENTED_EDGE('',*,*,#8935,.T.);
#12371=ORIENTED_EDGE('',*,*,#8933,.T.);
#12372=ORIENTED_EDGE('',*,*,#8935,.F.);
#12373=ORIENTED_EDGE('',*,*,#8936,.F.);
#12374=ORIENTED_EDGE('',*,*,#8937,.T.);
#12375=ORIENTED_EDGE('',*,*,#8934,.T.);
#12376=ORIENTED_EDGE('',*,*,#8937,.F.);
#12377=ORIENTED_EDGE('',*,*,#8938,.F.);
#12378=ORIENTED_EDGE('',*,*,#8939,.T.);
#12379=ORIENTED_EDGE('',*,*,#8936,.T.);
#12380=ORIENTED_EDGE('',*,*,#8939,.F.);
#12381=ORIENTED_EDGE('',*,*,#8938,.T.);
#12382=ORIENTED_EDGE('',*,*,#8940,.F.);
#12383=ORIENTED_EDGE('',*,*,#8940,.T.);
#12384=ORIENTED_EDGE('',*,*,#8941,.T.);
#12385=ORIENTED_EDGE('',*,*,#8942,.F.);
#12386=ORIENTED_EDGE('',*,*,#8941,.F.);
#12387=ORIENTED_EDGE('',*,*,#8942,.T.);
#12388=ORIENTED_EDGE('',*,*,#8943,.F.);
#12389=ORIENTED_EDGE('',*,*,#8944,.F.);
#12390=ORIENTED_EDGE('',*,*,#8945,.T.);
#12391=ORIENTED_EDGE('',*,*,#8943,.T.);
#12392=ORIENTED_EDGE('',*,*,#8945,.F.);
#12393=ORIENTED_EDGE('',*,*,#8944,.T.);
#12394=ORIENTED_EDGE('',*,*,#8946,.F.);
#12395=ORIENTED_EDGE('',*,*,#8946,.T.);
#12396=ORIENTED_EDGE('',*,*,#8947,.T.);
#12397=ORIENTED_EDGE('',*,*,#8948,.F.);
#12398=ORIENTED_EDGE('',*,*,#8947,.F.);
#12399=ORIENTED_EDGE('',*,*,#8948,.T.);
#12400=ORIENTED_EDGE('',*,*,#8949,.T.);
#12401=ORIENTED_EDGE('',*,*,#8950,.F.);
#12402=ORIENTED_EDGE('',*,*,#8949,.F.);
#12403=ORIENTED_EDGE('',*,*,#8950,.T.);
#12404=ORIENTED_EDGE('',*,*,#8951,.T.);
#12405=ORIENTED_EDGE('',*,*,#8952,.F.);
#12406=ORIENTED_EDGE('',*,*,#8951,.F.);
#12407=ORIENTED_EDGE('',*,*,#8929,.F.);
#12408=ORIENTED_EDGE('',*,*,#8952,.T.);
#12409=ORIENTED_EDGE('',*,*,#8953,.T.);
#12410=ORIENTED_EDGE('',*,*,#8954,.T.);
#12411=ORIENTED_EDGE('',*,*,#8955,.F.);
#12412=ORIENTED_EDGE('',*,*,#8954,.F.);
#12413=ORIENTED_EDGE('',*,*,#8956,.F.);
#12414=ORIENTED_EDGE('',*,*,#8955,.T.);
#12415=ORIENTED_EDGE('',*,*,#8957,.F.);
#12416=ORIENTED_EDGE('',*,*,#8953,.F.);
#12417=ORIENTED_EDGE('',*,*,#8958,.T.);
#12418=ORIENTED_EDGE('',*,*,#8959,.T.);
#12419=ORIENTED_EDGE('',*,*,#8957,.T.);
#12420=ORIENTED_EDGE('',*,*,#8959,.F.);
#12421=ORIENTED_EDGE('',*,*,#8960,.T.);
#12422=ORIENTED_EDGE('',*,*,#8961,.T.);
#12423=ORIENTED_EDGE('',*,*,#8962,.F.);
#12424=ORIENTED_EDGE('',*,*,#8961,.F.);
#12425=ORIENTED_EDGE('',*,*,#8963,.F.);
#12426=ORIENTED_EDGE('',*,*,#8962,.T.);
#12427=ORIENTED_EDGE('',*,*,#8964,.F.);
#12428=ORIENTED_EDGE('',*,*,#8965,.T.);
#12429=ORIENTED_EDGE('',*,*,#8963,.T.);
#12430=ORIENTED_EDGE('',*,*,#8965,.F.);
#12431=ORIENTED_EDGE('',*,*,#8964,.T.);
#12432=ORIENTED_EDGE('',*,*,#8966,.F.);
#12433=ORIENTED_EDGE('',*,*,#8966,.T.);
#12434=ORIENTED_EDGE('',*,*,#8967,.T.);
#12435=ORIENTED_EDGE('',*,*,#8968,.F.);
#12436=ORIENTED_EDGE('',*,*,#8967,.F.);
#12437=ORIENTED_EDGE('',*,*,#8958,.F.);
#12438=ORIENTED_EDGE('',*,*,#8968,.T.);
#12439=ORIENTED_EDGE('',*,*,#8956,.T.);
#12440=ORIENTED_EDGE('',*,*,#8969,.T.);
#12441=ORIENTED_EDGE('',*,*,#8970,.F.);
#12442=ORIENTED_EDGE('',*,*,#8969,.F.);
#12443=ORIENTED_EDGE('',*,*,#8970,.T.);
#12444=ORIENTED_EDGE('',*,*,#8960,.F.);
#12445=ORIENTED_EDGE('',*,*,#8971,.T.);
#12446=ORIENTED_EDGE('',*,*,#8972,.T.);
#12447=ORIENTED_EDGE('',*,*,#8973,.T.);
#12448=ORIENTED_EDGE('',*,*,#8974,.T.);
#12449=ORIENTED_EDGE('',*,*,#8973,.F.);
#12450=ORIENTED_EDGE('',*,*,#8975,.T.);
#12451=ORIENTED_EDGE('',*,*,#8974,.F.);
#12452=ORIENTED_EDGE('',*,*,#8971,.F.);
#12453=ORIENTED_EDGE('',*,*,#8972,.F.);
#12454=ORIENTED_EDGE('',*,*,#8976,.T.);
#12455=ORIENTED_EDGE('',*,*,#8977,.F.);
#12456=ORIENTED_EDGE('',*,*,#8976,.F.);
#12457=ORIENTED_EDGE('',*,*,#8978,.T.);
#12458=ORIENTED_EDGE('',*,*,#8979,.T.);
#12459=ORIENTED_EDGE('',*,*,#8980,.T.);
#12460=ORIENTED_EDGE('',*,*,#8981,.T.);
#12461=ORIENTED_EDGE('',*,*,#8980,.F.);
#12462=ORIENTED_EDGE('',*,*,#8981,.F.);
#12463=ORIENTED_EDGE('',*,*,#8982,.T.);
#12464=ORIENTED_EDGE('',*,*,#8983,.F.);
#12465=ORIENTED_EDGE('',*,*,#8984,.T.);
#12466=ORIENTED_EDGE('',*,*,#8978,.F.);
#12467=ORIENTED_EDGE('',*,*,#8979,.F.);
#12468=ORIENTED_EDGE('',*,*,#8984,.F.);
#12469=ORIENTED_EDGE('',*,*,#8985,.T.);
#12470=ORIENTED_EDGE('',*,*,#8986,.T.);
#12471=ORIENTED_EDGE('',*,*,#8982,.F.);
#12472=ORIENTED_EDGE('',*,*,#8986,.F.);
#12473=ORIENTED_EDGE('',*,*,#8987,.F.);
#12474=ORIENTED_EDGE('',*,*,#8983,.T.);
#12475=ORIENTED_EDGE('',*,*,#8975,.F.);
#12476=ORIENTED_EDGE('',*,*,#8988,.T.);
#12477=ORIENTED_EDGE('',*,*,#8987,.T.);
#12478=ORIENTED_EDGE('',*,*,#8988,.F.);
#12479=ORIENTED_EDGE('',*,*,#8977,.T.);
#12480=ORIENTED_EDGE('',*,*,#8989,.F.);
#12481=ORIENTED_EDGE('',*,*,#8989,.T.);
#12482=ORIENTED_EDGE('',*,*,#8990,.T.);
#12483=ORIENTED_EDGE('',*,*,#8985,.F.);
#12484=ORIENTED_EDGE('',*,*,#8990,.F.);
#12485=ORIENTED_EDGE('',*,*,#8991,.T.);
#12486=ORIENTED_EDGE('',*,*,#8992,.T.);
#12487=ORIENTED_EDGE('',*,*,#8993,.T.);
#12488=ORIENTED_EDGE('',*,*,#8992,.F.);
#12489=ORIENTED_EDGE('',*,*,#8994,.F.);
#12490=ORIENTED_EDGE('',*,*,#8995,.T.);
#12491=ORIENTED_EDGE('',*,*,#8993,.F.);
#12492=ORIENTED_EDGE('',*,*,#8995,.F.);
#12493=ORIENTED_EDGE('',*,*,#8996,.T.);
#12494=ORIENTED_EDGE('',*,*,#8991,.F.);
#12495=ORIENTED_EDGE('',*,*,#8997,.F.);
#12496=ORIENTED_EDGE('',*,*,#8998,.T.);
#12497=ORIENTED_EDGE('',*,*,#8999,.F.);
#12498=ORIENTED_EDGE('',*,*,#8998,.F.);
#12499=ORIENTED_EDGE('',*,*,#9000,.F.);
#12500=ORIENTED_EDGE('',*,*,#8994,.T.);
#12501=ORIENTED_EDGE('',*,*,#8999,.T.);
#12502=ORIENTED_EDGE('',*,*,#9001,.F.);
#12503=ORIENTED_EDGE('',*,*,#9002,.T.);
#12504=ORIENTED_EDGE('',*,*,#9003,.T.);
#12505=ORIENTED_EDGE('',*,*,#9004,.T.);
#12506=ORIENTED_EDGE('',*,*,#9002,.F.);
#12507=ORIENTED_EDGE('',*,*,#9005,.F.);
#12508=ORIENTED_EDGE('',*,*,#9001,.T.);
#12509=ORIENTED_EDGE('',*,*,#9006,.F.);
#12510=ORIENTED_EDGE('',*,*,#9007,.T.);
#12511=ORIENTED_EDGE('',*,*,#9005,.T.);
#12512=ORIENTED_EDGE('',*,*,#9007,.F.);
#12513=ORIENTED_EDGE('',*,*,#9008,.F.);
#12514=ORIENTED_EDGE('',*,*,#9009,.T.);
#12515=ORIENTED_EDGE('',*,*,#9006,.T.);
#12516=ORIENTED_EDGE('',*,*,#9009,.F.);
#12517=ORIENTED_EDGE('',*,*,#8996,.F.);
#12518=ORIENTED_EDGE('',*,*,#9010,.T.);
#12519=ORIENTED_EDGE('',*,*,#9008,.T.);
#12520=ORIENTED_EDGE('',*,*,#9010,.F.);
#12521=ORIENTED_EDGE('',*,*,#9003,.F.);
#12522=ORIENTED_EDGE('',*,*,#9004,.F.);
#12523=ORIENTED_EDGE('',*,*,#9011,.T.);
#12524=ORIENTED_EDGE('',*,*,#9000,.T.);
#12525=ORIENTED_EDGE('',*,*,#8997,.T.);
#12526=ORIENTED_EDGE('',*,*,#9011,.F.);
#12527=ORIENTED_EDGE('',*,*,#9012,.T.);
#12528=ORIENTED_EDGE('',*,*,#9013,.T.);
#12529=ORIENTED_EDGE('',*,*,#9014,.F.);
#12530=ORIENTED_EDGE('',*,*,#9013,.F.);
#12531=ORIENTED_EDGE('',*,*,#9015,.F.);
#12532=ORIENTED_EDGE('',*,*,#9014,.T.);
#12533=ORIENTED_EDGE('',*,*,#9016,.F.);
#12534=ORIENTED_EDGE('',*,*,#9017,.T.);
#12535=ORIENTED_EDGE('',*,*,#9015,.T.);
#12536=ORIENTED_EDGE('',*,*,#9017,.F.);
#12537=ORIENTED_EDGE('',*,*,#9018,.F.);
#12538=ORIENTED_EDGE('',*,*,#9019,.T.);
#12539=ORIENTED_EDGE('',*,*,#9016,.T.);
#12540=ORIENTED_EDGE('',*,*,#9019,.F.);
#12541=ORIENTED_EDGE('',*,*,#9018,.T.);
#12542=ORIENTED_EDGE('',*,*,#9020,.F.);
#12543=ORIENTED_EDGE('',*,*,#9021,.F.);
#12544=ORIENTED_EDGE('',*,*,#9022,.T.);
#12545=ORIENTED_EDGE('',*,*,#9020,.T.);
#12546=ORIENTED_EDGE('',*,*,#9022,.F.);
#12547=ORIENTED_EDGE('',*,*,#9021,.T.);
#12548=ORIENTED_EDGE('',*,*,#9023,.F.);
#12549=ORIENTED_EDGE('',*,*,#9024,.F.);
#12550=ORIENTED_EDGE('',*,*,#9025,.T.);
#12551=ORIENTED_EDGE('',*,*,#9025,.F.);
#12552=ORIENTED_EDGE('',*,*,#9026,.F.);
#12553=ORIENTED_EDGE('',*,*,#9027,.F.);
#12554=ORIENTED_EDGE('',*,*,#9028,.F.);
#12555=ORIENTED_EDGE('',*,*,#9028,.T.);
#12556=ORIENTED_EDGE('',*,*,#9023,.T.);
#12557=ORIENTED_EDGE('',*,*,#9024,.T.);
#12558=ORIENTED_EDGE('',*,*,#9027,.T.);
#12559=ORIENTED_EDGE('',*,*,#9029,.T.);
#12560=ORIENTED_EDGE('',*,*,#9030,.F.);
#12561=ORIENTED_EDGE('',*,*,#9029,.F.);
#12562=ORIENTED_EDGE('',*,*,#9026,.T.);
#12563=ORIENTED_EDGE('',*,*,#9012,.F.);
#12564=ORIENTED_EDGE('',*,*,#9030,.T.);
#12565=ORIENTED_EDGE('',*,*,#9031,.T.);
#12566=ORIENTED_EDGE('',*,*,#9032,.T.);
#12567=ORIENTED_EDGE('',*,*,#9033,.T.);
#12568=ORIENTED_EDGE('',*,*,#9034,.T.);
#12569=ORIENTED_EDGE('',*,*,#9032,.F.);
#12570=ORIENTED_EDGE('',*,*,#9031,.F.);
#12571=ORIENTED_EDGE('',*,*,#9035,.T.);
#12572=ORIENTED_EDGE('',*,*,#9036,.F.);
#12573=ORIENTED_EDGE('',*,*,#9037,.T.);
#12574=ORIENTED_EDGE('',*,*,#9038,.F.);
#12575=ORIENTED_EDGE('',*,*,#9039,.T.);
#12576=ORIENTED_EDGE('',*,*,#9040,.F.);
#12577=ORIENTED_EDGE('',*,*,#9041,.T.);
#12578=ORIENTED_EDGE('',*,*,#9042,.F.);
#12579=ORIENTED_EDGE('',*,*,#9043,.T.);
#12580=ORIENTED_EDGE('',*,*,#9044,.F.);
#12581=ORIENTED_EDGE('',*,*,#9045,.T.);
#12582=ORIENTED_EDGE('',*,*,#9046,.F.);
#12583=ORIENTED_EDGE('',*,*,#9047,.T.);
#12584=ORIENTED_EDGE('',*,*,#9048,.F.);
#12585=ORIENTED_EDGE('',*,*,#9033,.F.);
#12586=ORIENTED_EDGE('',*,*,#9034,.F.);
#12587=ORIENTED_EDGE('',*,*,#9049,.T.);
#12588=ORIENTED_EDGE('',*,*,#9050,.T.);
#12589=ORIENTED_EDGE('',*,*,#9049,.F.);
#12590=ORIENTED_EDGE('',*,*,#9051,.F.);
#12591=ORIENTED_EDGE('',*,*,#9052,.F.);
#12592=ORIENTED_EDGE('',*,*,#9035,.F.);
#12593=ORIENTED_EDGE('',*,*,#9053,.F.);
#12594=ORIENTED_EDGE('',*,*,#9052,.T.);
#12595=ORIENTED_EDGE('',*,*,#9054,.F.);
#12596=ORIENTED_EDGE('',*,*,#9055,.T.);
#12597=ORIENTED_EDGE('',*,*,#9036,.T.);
#12598=ORIENTED_EDGE('',*,*,#9056,.F.);
#12599=ORIENTED_EDGE('',*,*,#9057,.F.);
#12600=ORIENTED_EDGE('',*,*,#9037,.F.);
#12601=ORIENTED_EDGE('',*,*,#9055,.F.);
#12602=ORIENTED_EDGE('',*,*,#9057,.T.);
#12603=ORIENTED_EDGE('',*,*,#9058,.F.);
#12604=ORIENTED_EDGE('',*,*,#9059,.T.);
#12605=ORIENTED_EDGE('',*,*,#9038,.T.);
#12606=ORIENTED_EDGE('',*,*,#9060,.F.);
#12607=ORIENTED_EDGE('',*,*,#9061,.F.);
#12608=ORIENTED_EDGE('',*,*,#9039,.F.);
#12609=ORIENTED_EDGE('',*,*,#9059,.F.);
#12610=ORIENTED_EDGE('',*,*,#9061,.T.);
#12611=ORIENTED_EDGE('',*,*,#9062,.F.);
#12612=ORIENTED_EDGE('',*,*,#9063,.T.);
#12613=ORIENTED_EDGE('',*,*,#9040,.T.);
#12614=ORIENTED_EDGE('',*,*,#9064,.F.);
#12615=ORIENTED_EDGE('',*,*,#9065,.F.);
#12616=ORIENTED_EDGE('',*,*,#9041,.F.);
#12617=ORIENTED_EDGE('',*,*,#9063,.F.);
#12618=ORIENTED_EDGE('',*,*,#9065,.T.);
#12619=ORIENTED_EDGE('',*,*,#9066,.F.);
#12620=ORIENTED_EDGE('',*,*,#9067,.T.);
#12621=ORIENTED_EDGE('',*,*,#9042,.T.);
#12622=ORIENTED_EDGE('',*,*,#9068,.F.);
#12623=ORIENTED_EDGE('',*,*,#9069,.F.);
#12624=ORIENTED_EDGE('',*,*,#9043,.F.);
#12625=ORIENTED_EDGE('',*,*,#9067,.F.);
#12626=ORIENTED_EDGE('',*,*,#9069,.T.);
#12627=ORIENTED_EDGE('',*,*,#9070,.F.);
#12628=ORIENTED_EDGE('',*,*,#9071,.T.);
#12629=ORIENTED_EDGE('',*,*,#9044,.T.);
#12630=ORIENTED_EDGE('',*,*,#9072,.F.);
#12631=ORIENTED_EDGE('',*,*,#9073,.F.);
#12632=ORIENTED_EDGE('',*,*,#9045,.F.);
#12633=ORIENTED_EDGE('',*,*,#9071,.F.);
#12634=ORIENTED_EDGE('',*,*,#9073,.T.);
#12635=ORIENTED_EDGE('',*,*,#9074,.F.);
#12636=ORIENTED_EDGE('',*,*,#9075,.T.);
#12637=ORIENTED_EDGE('',*,*,#9046,.T.);
#12638=ORIENTED_EDGE('',*,*,#9075,.F.);
#12639=ORIENTED_EDGE('',*,*,#9076,.F.);
#12640=ORIENTED_EDGE('',*,*,#9077,.F.);
#12641=ORIENTED_EDGE('',*,*,#9047,.F.);
#12642=ORIENTED_EDGE('',*,*,#9078,.F.);
#12643=ORIENTED_EDGE('',*,*,#9051,.T.);
#12644=ORIENTED_EDGE('',*,*,#9079,.T.);
#12645=ORIENTED_EDGE('',*,*,#9076,.T.);
#12646=ORIENTED_EDGE('',*,*,#9074,.T.);
#12647=ORIENTED_EDGE('',*,*,#9072,.T.);
#12648=ORIENTED_EDGE('',*,*,#9070,.T.);
#12649=ORIENTED_EDGE('',*,*,#9068,.T.);
#12650=ORIENTED_EDGE('',*,*,#9066,.T.);
#12651=ORIENTED_EDGE('',*,*,#9064,.T.);
#12652=ORIENTED_EDGE('',*,*,#9062,.T.);
#12653=ORIENTED_EDGE('',*,*,#9060,.T.);
#12654=ORIENTED_EDGE('',*,*,#9058,.T.);
#12655=ORIENTED_EDGE('',*,*,#9056,.T.);
#12656=ORIENTED_EDGE('',*,*,#9054,.T.);
#12657=ORIENTED_EDGE('',*,*,#9053,.T.);
#12658=ORIENTED_EDGE('',*,*,#9048,.T.);
#12659=ORIENTED_EDGE('',*,*,#9077,.T.);
#12660=ORIENTED_EDGE('',*,*,#9079,.F.);
#12661=ORIENTED_EDGE('',*,*,#9050,.F.);
#12662=ORIENTED_EDGE('',*,*,#9080,.T.);
#12663=ORIENTED_EDGE('',*,*,#9078,.T.);
#12664=ORIENTED_EDGE('',*,*,#9080,.F.);
#12665=ORIENTED_EDGE('',*,*,#9081,.F.);
#12666=ORIENTED_EDGE('',*,*,#9082,.T.);
#12667=ORIENTED_EDGE('',*,*,#9083,.T.);
#12668=ORIENTED_EDGE('',*,*,#9084,.T.);
#12669=ORIENTED_EDGE('',*,*,#9085,.F.);
#12670=ORIENTED_EDGE('',*,*,#9086,.T.);
#12671=ORIENTED_EDGE('',*,*,#9081,.T.);
#12672=ORIENTED_EDGE('',*,*,#9087,.T.);
#12673=ORIENTED_EDGE('',*,*,#9088,.F.);
#12674=ORIENTED_EDGE('',*,*,#9089,.T.);
#12675=ORIENTED_EDGE('',*,*,#9085,.T.);
#12676=ORIENTED_EDGE('',*,*,#9090,.T.);
#12677=ORIENTED_EDGE('',*,*,#9091,.F.);
#12678=ORIENTED_EDGE('',*,*,#9092,.T.);
#12679=ORIENTED_EDGE('',*,*,#9088,.T.);
#12680=ORIENTED_EDGE('',*,*,#9093,.T.);
#12681=ORIENTED_EDGE('',*,*,#9094,.F.);
#12682=ORIENTED_EDGE('',*,*,#9095,.T.);
#12683=ORIENTED_EDGE('',*,*,#9091,.T.);
#12684=ORIENTED_EDGE('',*,*,#9096,.T.);
#12685=ORIENTED_EDGE('',*,*,#9097,.F.);
#12686=ORIENTED_EDGE('',*,*,#9098,.T.);
#12687=ORIENTED_EDGE('',*,*,#9094,.T.);
#12688=ORIENTED_EDGE('',*,*,#9099,.T.);
#12689=ORIENTED_EDGE('',*,*,#9100,.F.);
#12690=ORIENTED_EDGE('',*,*,#9101,.T.);
#12691=ORIENTED_EDGE('',*,*,#9097,.T.);
#12692=ORIENTED_EDGE('',*,*,#9102,.T.);
#12693=ORIENTED_EDGE('',*,*,#9103,.F.);
#12694=ORIENTED_EDGE('',*,*,#9104,.T.);
#12695=ORIENTED_EDGE('',*,*,#9100,.T.);
#12696=ORIENTED_EDGE('',*,*,#9105,.T.);
#12697=ORIENTED_EDGE('',*,*,#9106,.F.);
#12698=ORIENTED_EDGE('',*,*,#9107,.T.);
#12699=ORIENTED_EDGE('',*,*,#9103,.T.);
#12700=ORIENTED_EDGE('',*,*,#9108,.T.);
#12701=ORIENTED_EDGE('',*,*,#9109,.F.);
#12702=ORIENTED_EDGE('',*,*,#9110,.T.);
#12703=ORIENTED_EDGE('',*,*,#9106,.T.);
#12704=ORIENTED_EDGE('',*,*,#9111,.T.);
#12705=ORIENTED_EDGE('',*,*,#9112,.F.);
#12706=ORIENTED_EDGE('',*,*,#9113,.T.);
#12707=ORIENTED_EDGE('',*,*,#9109,.T.);
#12708=ORIENTED_EDGE('',*,*,#9114,.T.);
#12709=ORIENTED_EDGE('',*,*,#9115,.F.);
#12710=ORIENTED_EDGE('',*,*,#9116,.T.);
#12711=ORIENTED_EDGE('',*,*,#9112,.T.);
#12712=ORIENTED_EDGE('',*,*,#9117,.T.);
#12713=ORIENTED_EDGE('',*,*,#9118,.F.);
#12714=ORIENTED_EDGE('',*,*,#9119,.T.);
#12715=ORIENTED_EDGE('',*,*,#9115,.T.);
#12716=ORIENTED_EDGE('',*,*,#9120,.T.);
#12717=ORIENTED_EDGE('',*,*,#9121,.F.);
#12718=ORIENTED_EDGE('',*,*,#9122,.T.);
#12719=ORIENTED_EDGE('',*,*,#9118,.T.);
#12720=ORIENTED_EDGE('',*,*,#9123,.T.);
#12721=ORIENTED_EDGE('',*,*,#9124,.F.);
#12722=ORIENTED_EDGE('',*,*,#9125,.T.);
#12723=ORIENTED_EDGE('',*,*,#9121,.T.);
#12724=ORIENTED_EDGE('',*,*,#9126,.T.);
#12725=ORIENTED_EDGE('',*,*,#9127,.F.);
#12726=ORIENTED_EDGE('',*,*,#9128,.T.);
#12727=ORIENTED_EDGE('',*,*,#9124,.T.);
#12728=ORIENTED_EDGE('',*,*,#9129,.T.);
#12729=ORIENTED_EDGE('',*,*,#9130,.F.);
#12730=ORIENTED_EDGE('',*,*,#9131,.T.);
#12731=ORIENTED_EDGE('',*,*,#9127,.T.);
#12732=ORIENTED_EDGE('',*,*,#9132,.T.);
#12733=ORIENTED_EDGE('',*,*,#9133,.F.);
#12734=ORIENTED_EDGE('',*,*,#9134,.T.);
#12735=ORIENTED_EDGE('',*,*,#9130,.T.);
#12736=ORIENTED_EDGE('',*,*,#9135,.T.);
#12737=ORIENTED_EDGE('',*,*,#9136,.F.);
#12738=ORIENTED_EDGE('',*,*,#9137,.T.);
#12739=ORIENTED_EDGE('',*,*,#9133,.T.);
#12740=ORIENTED_EDGE('',*,*,#9138,.T.);
#12741=ORIENTED_EDGE('',*,*,#9139,.F.);
#12742=ORIENTED_EDGE('',*,*,#9140,.T.);
#12743=ORIENTED_EDGE('',*,*,#9136,.T.);
#12744=ORIENTED_EDGE('',*,*,#9141,.T.);
#12745=ORIENTED_EDGE('',*,*,#9142,.F.);
#12746=ORIENTED_EDGE('',*,*,#9143,.T.);
#12747=ORIENTED_EDGE('',*,*,#9139,.T.);
#12748=ORIENTED_EDGE('',*,*,#9144,.T.);
#12749=ORIENTED_EDGE('',*,*,#9145,.F.);
#12750=ORIENTED_EDGE('',*,*,#9146,.T.);
#12751=ORIENTED_EDGE('',*,*,#9142,.T.);
#12752=ORIENTED_EDGE('',*,*,#9147,.T.);
#12753=ORIENTED_EDGE('',*,*,#9148,.F.);
#12754=ORIENTED_EDGE('',*,*,#9149,.T.);
#12755=ORIENTED_EDGE('',*,*,#9145,.T.);
#12756=ORIENTED_EDGE('',*,*,#9150,.T.);
#12757=ORIENTED_EDGE('',*,*,#9151,.F.);
#12758=ORIENTED_EDGE('',*,*,#9152,.T.);
#12759=ORIENTED_EDGE('',*,*,#9148,.T.);
#12760=ORIENTED_EDGE('',*,*,#9153,.T.);
#12761=ORIENTED_EDGE('',*,*,#9154,.F.);
#12762=ORIENTED_EDGE('',*,*,#9155,.T.);
#12763=ORIENTED_EDGE('',*,*,#9151,.T.);
#12764=ORIENTED_EDGE('',*,*,#9156,.T.);
#12765=ORIENTED_EDGE('',*,*,#9157,.F.);
#12766=ORIENTED_EDGE('',*,*,#9158,.T.);
#12767=ORIENTED_EDGE('',*,*,#9154,.T.);
#12768=ORIENTED_EDGE('',*,*,#9159,.T.);
#12769=ORIENTED_EDGE('',*,*,#9160,.F.);
#12770=ORIENTED_EDGE('',*,*,#9161,.T.);
#12771=ORIENTED_EDGE('',*,*,#9157,.T.);
#12772=ORIENTED_EDGE('',*,*,#9162,.T.);
#12773=ORIENTED_EDGE('',*,*,#9163,.F.);
#12774=ORIENTED_EDGE('',*,*,#9164,.T.);
#12775=ORIENTED_EDGE('',*,*,#9160,.T.);
#12776=ORIENTED_EDGE('',*,*,#9165,.T.);
#12777=ORIENTED_EDGE('',*,*,#9166,.F.);
#12778=ORIENTED_EDGE('',*,*,#9167,.T.);
#12779=ORIENTED_EDGE('',*,*,#9163,.T.);
#12780=ORIENTED_EDGE('',*,*,#9168,.T.);
#12781=ORIENTED_EDGE('',*,*,#9169,.F.);
#12782=ORIENTED_EDGE('',*,*,#9170,.T.);
#12783=ORIENTED_EDGE('',*,*,#9166,.T.);
#12784=ORIENTED_EDGE('',*,*,#9171,.T.);
#12785=ORIENTED_EDGE('',*,*,#9172,.F.);
#12786=ORIENTED_EDGE('',*,*,#9173,.T.);
#12787=ORIENTED_EDGE('',*,*,#9169,.T.);
#12788=ORIENTED_EDGE('',*,*,#9174,.T.);
#12789=ORIENTED_EDGE('',*,*,#9175,.F.);
#12790=ORIENTED_EDGE('',*,*,#9176,.T.);
#12791=ORIENTED_EDGE('',*,*,#9172,.T.);
#12792=ORIENTED_EDGE('',*,*,#9177,.T.);
#12793=ORIENTED_EDGE('',*,*,#9178,.F.);
#12794=ORIENTED_EDGE('',*,*,#9179,.T.);
#12795=ORIENTED_EDGE('',*,*,#9175,.T.);
#12796=ORIENTED_EDGE('',*,*,#9180,.T.);
#12797=ORIENTED_EDGE('',*,*,#9181,.F.);
#12798=ORIENTED_EDGE('',*,*,#9182,.T.);
#12799=ORIENTED_EDGE('',*,*,#9178,.T.);
#12800=ORIENTED_EDGE('',*,*,#9183,.T.);
#12801=ORIENTED_EDGE('',*,*,#9184,.F.);
#12802=ORIENTED_EDGE('',*,*,#9185,.T.);
#12803=ORIENTED_EDGE('',*,*,#9186,.F.);
#12804=ORIENTED_EDGE('',*,*,#9187,.F.);
#12805=ORIENTED_EDGE('',*,*,#9188,.F.);
#12806=ORIENTED_EDGE('',*,*,#9189,.T.);
#12807=ORIENTED_EDGE('',*,*,#9184,.T.);
#12808=ORIENTED_EDGE('',*,*,#9190,.F.);
#12809=ORIENTED_EDGE('',*,*,#9191,.F.);
#12810=ORIENTED_EDGE('',*,*,#9192,.T.);
#12811=ORIENTED_EDGE('',*,*,#9188,.T.);
#12812=ORIENTED_EDGE('',*,*,#9193,.F.);
#12813=ORIENTED_EDGE('',*,*,#9194,.F.);
#12814=ORIENTED_EDGE('',*,*,#9195,.T.);
#12815=ORIENTED_EDGE('',*,*,#9191,.T.);
#12816=ORIENTED_EDGE('',*,*,#9196,.F.);
#12817=ORIENTED_EDGE('',*,*,#9197,.F.);
#12818=ORIENTED_EDGE('',*,*,#9198,.T.);
#12819=ORIENTED_EDGE('',*,*,#9194,.T.);
#12820=ORIENTED_EDGE('',*,*,#9199,.F.);
#12821=ORIENTED_EDGE('',*,*,#9200,.F.);
#12822=ORIENTED_EDGE('',*,*,#9201,.T.);
#12823=ORIENTED_EDGE('',*,*,#9197,.T.);
#12824=ORIENTED_EDGE('',*,*,#9202,.F.);
#12825=ORIENTED_EDGE('',*,*,#9203,.F.);
#12826=ORIENTED_EDGE('',*,*,#9204,.T.);
#12827=ORIENTED_EDGE('',*,*,#9200,.T.);
#12828=ORIENTED_EDGE('',*,*,#9205,.F.);
#12829=ORIENTED_EDGE('',*,*,#9206,.F.);
#12830=ORIENTED_EDGE('',*,*,#9207,.T.);
#12831=ORIENTED_EDGE('',*,*,#9203,.T.);
#12832=ORIENTED_EDGE('',*,*,#9208,.F.);
#12833=ORIENTED_EDGE('',*,*,#9209,.F.);
#12834=ORIENTED_EDGE('',*,*,#9210,.T.);
#12835=ORIENTED_EDGE('',*,*,#9206,.T.);
#12836=ORIENTED_EDGE('',*,*,#9211,.F.);
#12837=ORIENTED_EDGE('',*,*,#9212,.F.);
#12838=ORIENTED_EDGE('',*,*,#9213,.T.);
#12839=ORIENTED_EDGE('',*,*,#9209,.T.);
#12840=ORIENTED_EDGE('',*,*,#9214,.F.);
#12841=ORIENTED_EDGE('',*,*,#9215,.F.);
#12842=ORIENTED_EDGE('',*,*,#9216,.T.);
#12843=ORIENTED_EDGE('',*,*,#9212,.T.);
#12844=ORIENTED_EDGE('',*,*,#9217,.F.);
#12845=ORIENTED_EDGE('',*,*,#9218,.F.);
#12846=ORIENTED_EDGE('',*,*,#9219,.T.);
#12847=ORIENTED_EDGE('',*,*,#9215,.T.);
#12848=ORIENTED_EDGE('',*,*,#9220,.F.);
#12849=ORIENTED_EDGE('',*,*,#9221,.F.);
#12850=ORIENTED_EDGE('',*,*,#9222,.T.);
#12851=ORIENTED_EDGE('',*,*,#9218,.T.);
#12852=ORIENTED_EDGE('',*,*,#9223,.F.);
#12853=ORIENTED_EDGE('',*,*,#9224,.F.);
#12854=ORIENTED_EDGE('',*,*,#9225,.T.);
#12855=ORIENTED_EDGE('',*,*,#9221,.T.);
#12856=ORIENTED_EDGE('',*,*,#9226,.F.);
#12857=ORIENTED_EDGE('',*,*,#9227,.F.);
#12858=ORIENTED_EDGE('',*,*,#9228,.T.);
#12859=ORIENTED_EDGE('',*,*,#9224,.T.);
#12860=ORIENTED_EDGE('',*,*,#9229,.F.);
#12861=ORIENTED_EDGE('',*,*,#9230,.F.);
#12862=ORIENTED_EDGE('',*,*,#9231,.T.);
#12863=ORIENTED_EDGE('',*,*,#9227,.T.);
#12864=ORIENTED_EDGE('',*,*,#9232,.F.);
#12865=ORIENTED_EDGE('',*,*,#9233,.F.);
#12866=ORIENTED_EDGE('',*,*,#9234,.T.);
#12867=ORIENTED_EDGE('',*,*,#9230,.T.);
#12868=ORIENTED_EDGE('',*,*,#9235,.F.);
#12869=ORIENTED_EDGE('',*,*,#9236,.F.);
#12870=ORIENTED_EDGE('',*,*,#9237,.T.);
#12871=ORIENTED_EDGE('',*,*,#9233,.T.);
#12872=ORIENTED_EDGE('',*,*,#9238,.F.);
#12873=ORIENTED_EDGE('',*,*,#9239,.F.);
#12874=ORIENTED_EDGE('',*,*,#9240,.T.);
#12875=ORIENTED_EDGE('',*,*,#9236,.T.);
#12876=ORIENTED_EDGE('',*,*,#9241,.F.);
#12877=ORIENTED_EDGE('',*,*,#9242,.F.);
#12878=ORIENTED_EDGE('',*,*,#9243,.T.);
#12879=ORIENTED_EDGE('',*,*,#9239,.T.);
#12880=ORIENTED_EDGE('',*,*,#9244,.F.);
#12881=ORIENTED_EDGE('',*,*,#9245,.F.);
#12882=ORIENTED_EDGE('',*,*,#9246,.T.);
#12883=ORIENTED_EDGE('',*,*,#9242,.T.);
#12884=ORIENTED_EDGE('',*,*,#9247,.F.);
#12885=ORIENTED_EDGE('',*,*,#9248,.F.);
#12886=ORIENTED_EDGE('',*,*,#9249,.T.);
#12887=ORIENTED_EDGE('',*,*,#9245,.T.);
#12888=ORIENTED_EDGE('',*,*,#9250,.F.);
#12889=ORIENTED_EDGE('',*,*,#9251,.F.);
#12890=ORIENTED_EDGE('',*,*,#9252,.T.);
#12891=ORIENTED_EDGE('',*,*,#9248,.T.);
#12892=ORIENTED_EDGE('',*,*,#9253,.F.);
#12893=ORIENTED_EDGE('',*,*,#9254,.F.);
#12894=ORIENTED_EDGE('',*,*,#9255,.T.);
#12895=ORIENTED_EDGE('',*,*,#9251,.T.);
#12896=ORIENTED_EDGE('',*,*,#9256,.F.);
#12897=ORIENTED_EDGE('',*,*,#9257,.F.);
#12898=ORIENTED_EDGE('',*,*,#9258,.T.);
#12899=ORIENTED_EDGE('',*,*,#9254,.T.);
#12900=ORIENTED_EDGE('',*,*,#9259,.F.);
#12901=ORIENTED_EDGE('',*,*,#9260,.F.);
#12902=ORIENTED_EDGE('',*,*,#9261,.T.);
#12903=ORIENTED_EDGE('',*,*,#9257,.T.);
#12904=ORIENTED_EDGE('',*,*,#9262,.F.);
#12905=ORIENTED_EDGE('',*,*,#9263,.F.);
#12906=ORIENTED_EDGE('',*,*,#9264,.T.);
#12907=ORIENTED_EDGE('',*,*,#9260,.T.);
#12908=ORIENTED_EDGE('',*,*,#9265,.F.);
#12909=ORIENTED_EDGE('',*,*,#9266,.F.);
#12910=ORIENTED_EDGE('',*,*,#9267,.T.);
#12911=ORIENTED_EDGE('',*,*,#9263,.T.);
#12912=ORIENTED_EDGE('',*,*,#9268,.F.);
#12913=ORIENTED_EDGE('',*,*,#9269,.F.);
#12914=ORIENTED_EDGE('',*,*,#9270,.T.);
#12915=ORIENTED_EDGE('',*,*,#9266,.T.);
#12916=ORIENTED_EDGE('',*,*,#9271,.F.);
#12917=ORIENTED_EDGE('',*,*,#9272,.F.);
#12918=ORIENTED_EDGE('',*,*,#9273,.T.);
#12919=ORIENTED_EDGE('',*,*,#9269,.T.);
#12920=ORIENTED_EDGE('',*,*,#9274,.F.);
#12921=ORIENTED_EDGE('',*,*,#9275,.F.);
#12922=ORIENTED_EDGE('',*,*,#9276,.T.);
#12923=ORIENTED_EDGE('',*,*,#9272,.T.);
#12924=ORIENTED_EDGE('',*,*,#9277,.F.);
#12925=ORIENTED_EDGE('',*,*,#9278,.F.);
#12926=ORIENTED_EDGE('',*,*,#9279,.T.);
#12927=ORIENTED_EDGE('',*,*,#9275,.T.);
#12928=ORIENTED_EDGE('',*,*,#9280,.F.);
#12929=ORIENTED_EDGE('',*,*,#9281,.F.);
#12930=ORIENTED_EDGE('',*,*,#9282,.T.);
#12931=ORIENTED_EDGE('',*,*,#9278,.T.);
#12932=ORIENTED_EDGE('',*,*,#9283,.F.);
#12933=ORIENTED_EDGE('',*,*,#9284,.F.);
#12934=ORIENTED_EDGE('',*,*,#9285,.T.);
#12935=ORIENTED_EDGE('',*,*,#9281,.T.);
#12936=ORIENTED_EDGE('',*,*,#9286,.F.);
#12937=ORIENTED_EDGE('',*,*,#9287,.F.);
#12938=ORIENTED_EDGE('',*,*,#9288,.F.);
#12939=ORIENTED_EDGE('',*,*,#9183,.F.);
#12940=ORIENTED_EDGE('',*,*,#9180,.F.);
#12941=ORIENTED_EDGE('',*,*,#9177,.F.);
#12942=ORIENTED_EDGE('',*,*,#9174,.F.);
#12943=ORIENTED_EDGE('',*,*,#9171,.F.);
#12944=ORIENTED_EDGE('',*,*,#9168,.F.);
#12945=ORIENTED_EDGE('',*,*,#9165,.F.);
#12946=ORIENTED_EDGE('',*,*,#9162,.F.);
#12947=ORIENTED_EDGE('',*,*,#9159,.F.);
#12948=ORIENTED_EDGE('',*,*,#9156,.F.);
#12949=ORIENTED_EDGE('',*,*,#9153,.F.);
#12950=ORIENTED_EDGE('',*,*,#9150,.F.);
#12951=ORIENTED_EDGE('',*,*,#9147,.F.);
#12952=ORIENTED_EDGE('',*,*,#9144,.F.);
#12953=ORIENTED_EDGE('',*,*,#9141,.F.);
#12954=ORIENTED_EDGE('',*,*,#9138,.F.);
#12955=ORIENTED_EDGE('',*,*,#9135,.F.);
#12956=ORIENTED_EDGE('',*,*,#9132,.F.);
#12957=ORIENTED_EDGE('',*,*,#9129,.F.);
#12958=ORIENTED_EDGE('',*,*,#9126,.F.);
#12959=ORIENTED_EDGE('',*,*,#9123,.F.);
#12960=ORIENTED_EDGE('',*,*,#9120,.F.);
#12961=ORIENTED_EDGE('',*,*,#9117,.F.);
#12962=ORIENTED_EDGE('',*,*,#9114,.F.);
#12963=ORIENTED_EDGE('',*,*,#9111,.F.);
#12964=ORIENTED_EDGE('',*,*,#9108,.F.);
#12965=ORIENTED_EDGE('',*,*,#9105,.F.);
#12966=ORIENTED_EDGE('',*,*,#9102,.F.);
#12967=ORIENTED_EDGE('',*,*,#9099,.F.);
#12968=ORIENTED_EDGE('',*,*,#9096,.F.);
#12969=ORIENTED_EDGE('',*,*,#9093,.F.);
#12970=ORIENTED_EDGE('',*,*,#9090,.F.);
#12971=ORIENTED_EDGE('',*,*,#9087,.F.);
#12972=ORIENTED_EDGE('',*,*,#9084,.F.);
#12973=ORIENTED_EDGE('',*,*,#9289,.F.);
#12974=ORIENTED_EDGE('',*,*,#9290,.T.);
#12975=ORIENTED_EDGE('',*,*,#9286,.T.);
#12976=ORIENTED_EDGE('',*,*,#9283,.T.);
#12977=ORIENTED_EDGE('',*,*,#9280,.T.);
#12978=ORIENTED_EDGE('',*,*,#9277,.T.);
#12979=ORIENTED_EDGE('',*,*,#9274,.T.);
#12980=ORIENTED_EDGE('',*,*,#9271,.T.);
#12981=ORIENTED_EDGE('',*,*,#9268,.T.);
#12982=ORIENTED_EDGE('',*,*,#9265,.T.);
#12983=ORIENTED_EDGE('',*,*,#9262,.T.);
#12984=ORIENTED_EDGE('',*,*,#9259,.T.);
#12985=ORIENTED_EDGE('',*,*,#9256,.T.);
#12986=ORIENTED_EDGE('',*,*,#9253,.T.);
#12987=ORIENTED_EDGE('',*,*,#9250,.T.);
#12988=ORIENTED_EDGE('',*,*,#9247,.T.);
#12989=ORIENTED_EDGE('',*,*,#9244,.T.);
#12990=ORIENTED_EDGE('',*,*,#9241,.T.);
#12991=ORIENTED_EDGE('',*,*,#9238,.T.);
#12992=ORIENTED_EDGE('',*,*,#9235,.T.);
#12993=ORIENTED_EDGE('',*,*,#9232,.T.);
#12994=ORIENTED_EDGE('',*,*,#9229,.T.);
#12995=ORIENTED_EDGE('',*,*,#9226,.T.);
#12996=ORIENTED_EDGE('',*,*,#9223,.T.);
#12997=ORIENTED_EDGE('',*,*,#9220,.T.);
#12998=ORIENTED_EDGE('',*,*,#9217,.T.);
#12999=ORIENTED_EDGE('',*,*,#9214,.T.);
#13000=ORIENTED_EDGE('',*,*,#9211,.T.);
#13001=ORIENTED_EDGE('',*,*,#9208,.T.);
#13002=ORIENTED_EDGE('',*,*,#9205,.T.);
#13003=ORIENTED_EDGE('',*,*,#9202,.T.);
#13004=ORIENTED_EDGE('',*,*,#9199,.T.);
#13005=ORIENTED_EDGE('',*,*,#9196,.T.);
#13006=ORIENTED_EDGE('',*,*,#9193,.T.);
#13007=ORIENTED_EDGE('',*,*,#9190,.T.);
#13008=ORIENTED_EDGE('',*,*,#9187,.T.);
#13009=ORIENTED_EDGE('',*,*,#9291,.T.);
#13010=ORIENTED_EDGE('',*,*,#9292,.T.);
#13011=ORIENTED_EDGE('',*,*,#9293,.T.);
#13012=ORIENTED_EDGE('',*,*,#9294,.T.);
#13013=ORIENTED_EDGE('',*,*,#9289,.T.);
#13014=ORIENTED_EDGE('',*,*,#9284,.T.);
#13015=ORIENTED_EDGE('',*,*,#9290,.F.);
#13016=ORIENTED_EDGE('',*,*,#9294,.F.);
#13017=ORIENTED_EDGE('',*,*,#9295,.T.);
#13018=ORIENTED_EDGE('',*,*,#9296,.F.);
#13019=ORIENTED_EDGE('',*,*,#9185,.F.);
#13020=ORIENTED_EDGE('',*,*,#9189,.F.);
#13021=ORIENTED_EDGE('',*,*,#9192,.F.);
#13022=ORIENTED_EDGE('',*,*,#9195,.F.);
#13023=ORIENTED_EDGE('',*,*,#9198,.F.);
#13024=ORIENTED_EDGE('',*,*,#9201,.F.);
#13025=ORIENTED_EDGE('',*,*,#9204,.F.);
#13026=ORIENTED_EDGE('',*,*,#9207,.F.);
#13027=ORIENTED_EDGE('',*,*,#9210,.F.);
#13028=ORIENTED_EDGE('',*,*,#9213,.F.);
#13029=ORIENTED_EDGE('',*,*,#9216,.F.);
#13030=ORIENTED_EDGE('',*,*,#9219,.F.);
#13031=ORIENTED_EDGE('',*,*,#9222,.F.);
#13032=ORIENTED_EDGE('',*,*,#9225,.F.);
#13033=ORIENTED_EDGE('',*,*,#9228,.F.);
#13034=ORIENTED_EDGE('',*,*,#9231,.F.);
#13035=ORIENTED_EDGE('',*,*,#9234,.F.);
#13036=ORIENTED_EDGE('',*,*,#9237,.F.);
#13037=ORIENTED_EDGE('',*,*,#9240,.F.);
#13038=ORIENTED_EDGE('',*,*,#9243,.F.);
#13039=ORIENTED_EDGE('',*,*,#9246,.F.);
#13040=ORIENTED_EDGE('',*,*,#9249,.F.);
#13041=ORIENTED_EDGE('',*,*,#9252,.F.);
#13042=ORIENTED_EDGE('',*,*,#9255,.F.);
#13043=ORIENTED_EDGE('',*,*,#9258,.F.);
#13044=ORIENTED_EDGE('',*,*,#9261,.F.);
#13045=ORIENTED_EDGE('',*,*,#9264,.F.);
#13046=ORIENTED_EDGE('',*,*,#9267,.F.);
#13047=ORIENTED_EDGE('',*,*,#9270,.F.);
#13048=ORIENTED_EDGE('',*,*,#9273,.F.);
#13049=ORIENTED_EDGE('',*,*,#9276,.F.);
#13050=ORIENTED_EDGE('',*,*,#9279,.F.);
#13051=ORIENTED_EDGE('',*,*,#9282,.F.);
#13052=ORIENTED_EDGE('',*,*,#9285,.F.);
#13053=ORIENTED_EDGE('',*,*,#9295,.F.);
#13054=ORIENTED_EDGE('',*,*,#9293,.F.);
#13055=ORIENTED_EDGE('',*,*,#9082,.F.);
#13056=ORIENTED_EDGE('',*,*,#9086,.F.);
#13057=ORIENTED_EDGE('',*,*,#9089,.F.);
#13058=ORIENTED_EDGE('',*,*,#9092,.F.);
#13059=ORIENTED_EDGE('',*,*,#9095,.F.);
#13060=ORIENTED_EDGE('',*,*,#9098,.F.);
#13061=ORIENTED_EDGE('',*,*,#9101,.F.);
#13062=ORIENTED_EDGE('',*,*,#9104,.F.);
#13063=ORIENTED_EDGE('',*,*,#9107,.F.);
#13064=ORIENTED_EDGE('',*,*,#9110,.F.);
#13065=ORIENTED_EDGE('',*,*,#9113,.F.);
#13066=ORIENTED_EDGE('',*,*,#9116,.F.);
#13067=ORIENTED_EDGE('',*,*,#9119,.F.);
#13068=ORIENTED_EDGE('',*,*,#9122,.F.);
#13069=ORIENTED_EDGE('',*,*,#9125,.F.);
#13070=ORIENTED_EDGE('',*,*,#9128,.F.);
#13071=ORIENTED_EDGE('',*,*,#9131,.F.);
#13072=ORIENTED_EDGE('',*,*,#9134,.F.);
#13073=ORIENTED_EDGE('',*,*,#9137,.F.);
#13074=ORIENTED_EDGE('',*,*,#9140,.F.);
#13075=ORIENTED_EDGE('',*,*,#9143,.F.);
#13076=ORIENTED_EDGE('',*,*,#9146,.F.);
#13077=ORIENTED_EDGE('',*,*,#9149,.F.);
#13078=ORIENTED_EDGE('',*,*,#9152,.F.);
#13079=ORIENTED_EDGE('',*,*,#9155,.F.);
#13080=ORIENTED_EDGE('',*,*,#9158,.F.);
#13081=ORIENTED_EDGE('',*,*,#9161,.F.);
#13082=ORIENTED_EDGE('',*,*,#9164,.F.);
#13083=ORIENTED_EDGE('',*,*,#9167,.F.);
#13084=ORIENTED_EDGE('',*,*,#9170,.F.);
#13085=ORIENTED_EDGE('',*,*,#9173,.F.);
#13086=ORIENTED_EDGE('',*,*,#9176,.F.);
#13087=ORIENTED_EDGE('',*,*,#9179,.F.);
#13088=ORIENTED_EDGE('',*,*,#9182,.F.);
#13089=ORIENTED_EDGE('',*,*,#9297,.F.);
#13090=ORIENTED_EDGE('',*,*,#9298,.F.);
#13091=ORIENTED_EDGE('',*,*,#9299,.T.);
#13092=ORIENTED_EDGE('',*,*,#9300,.F.);
#13093=ORIENTED_EDGE('',*,*,#9301,.F.);
#13094=ORIENTED_EDGE('',*,*,#9302,.F.);
#13095=ORIENTED_EDGE('',*,*,#9301,.T.);
#13096=ORIENTED_EDGE('',*,*,#9303,.T.);
#13097=ORIENTED_EDGE('',*,*,#9304,.F.);
#13098=ORIENTED_EDGE('',*,*,#9303,.F.);
#13099=ORIENTED_EDGE('',*,*,#9300,.T.);
#13100=ORIENTED_EDGE('',*,*,#9305,.T.);
#13101=ORIENTED_EDGE('',*,*,#9306,.F.);
#13102=ORIENTED_EDGE('',*,*,#9305,.F.);
#13103=ORIENTED_EDGE('',*,*,#9299,.F.);
#13104=ORIENTED_EDGE('',*,*,#9307,.F.);
#13105=ORIENTED_EDGE('',*,*,#9308,.T.);
#13106=ORIENTED_EDGE('',*,*,#9309,.F.);
#13107=ORIENTED_EDGE('',*,*,#9310,.F.);
#13108=ORIENTED_EDGE('',*,*,#9311,.F.);
#13109=ORIENTED_EDGE('',*,*,#9310,.T.);
#13110=ORIENTED_EDGE('',*,*,#9312,.T.);
#13111=ORIENTED_EDGE('',*,*,#9313,.F.);
#13112=ORIENTED_EDGE('',*,*,#9312,.F.);
#13113=ORIENTED_EDGE('',*,*,#9309,.T.);
#13114=ORIENTED_EDGE('',*,*,#9314,.T.);
#13115=ORIENTED_EDGE('',*,*,#9315,.F.);
#13116=ORIENTED_EDGE('',*,*,#9314,.F.);
#13117=ORIENTED_EDGE('',*,*,#9308,.F.);
#13118=ORIENTED_EDGE('',*,*,#9316,.F.);
#13119=ORIENTED_EDGE('',*,*,#9317,.T.);
#13120=ORIENTED_EDGE('',*,*,#9318,.F.);
#13121=ORIENTED_EDGE('',*,*,#9319,.F.);
#13122=ORIENTED_EDGE('',*,*,#9320,.F.);
#13123=ORIENTED_EDGE('',*,*,#9319,.T.);
#13124=ORIENTED_EDGE('',*,*,#9321,.T.);
#13125=ORIENTED_EDGE('',*,*,#9322,.F.);
#13126=ORIENTED_EDGE('',*,*,#9321,.F.);
#13127=ORIENTED_EDGE('',*,*,#9318,.T.);
#13128=ORIENTED_EDGE('',*,*,#9323,.T.);
#13129=ORIENTED_EDGE('',*,*,#9324,.F.);
#13130=ORIENTED_EDGE('',*,*,#9323,.F.);
#13131=ORIENTED_EDGE('',*,*,#9317,.F.);
#13132=ORIENTED_EDGE('',*,*,#9325,.F.);
#13133=ORIENTED_EDGE('',*,*,#9326,.T.);
#13134=ORIENTED_EDGE('',*,*,#9327,.F.);
#13135=ORIENTED_EDGE('',*,*,#9328,.F.);
#13136=ORIENTED_EDGE('',*,*,#9329,.F.);
#13137=ORIENTED_EDGE('',*,*,#9328,.T.);
#13138=ORIENTED_EDGE('',*,*,#9330,.T.);
#13139=ORIENTED_EDGE('',*,*,#9331,.F.);
#13140=ORIENTED_EDGE('',*,*,#9330,.F.);
#13141=ORIENTED_EDGE('',*,*,#9327,.T.);
#13142=ORIENTED_EDGE('',*,*,#9332,.T.);
#13143=ORIENTED_EDGE('',*,*,#9333,.F.);
#13144=ORIENTED_EDGE('',*,*,#9332,.F.);
#13145=ORIENTED_EDGE('',*,*,#9326,.F.);
#13146=ORIENTED_EDGE('',*,*,#9334,.F.);
#13147=ORIENTED_EDGE('',*,*,#9335,.T.);
#13148=ORIENTED_EDGE('',*,*,#9336,.F.);
#13149=ORIENTED_EDGE('',*,*,#9337,.F.);
#13150=ORIENTED_EDGE('',*,*,#9338,.F.);
#13151=ORIENTED_EDGE('',*,*,#9337,.T.);
#13152=ORIENTED_EDGE('',*,*,#9339,.T.);
#13153=ORIENTED_EDGE('',*,*,#9340,.F.);
#13154=ORIENTED_EDGE('',*,*,#9339,.F.);
#13155=ORIENTED_EDGE('',*,*,#9336,.T.);
#13156=ORIENTED_EDGE('',*,*,#9341,.T.);
#13157=ORIENTED_EDGE('',*,*,#9342,.F.);
#13158=ORIENTED_EDGE('',*,*,#9341,.F.);
#13159=ORIENTED_EDGE('',*,*,#9335,.F.);
#13160=ORIENTED_EDGE('',*,*,#9343,.F.);
#13161=ORIENTED_EDGE('',*,*,#9344,.T.);
#13162=ORIENTED_EDGE('',*,*,#9345,.F.);
#13163=ORIENTED_EDGE('',*,*,#9346,.F.);
#13164=ORIENTED_EDGE('',*,*,#9347,.F.);
#13165=ORIENTED_EDGE('',*,*,#9346,.T.);
#13166=ORIENTED_EDGE('',*,*,#9348,.T.);
#13167=ORIENTED_EDGE('',*,*,#9349,.F.);
#13168=ORIENTED_EDGE('',*,*,#9348,.F.);
#13169=ORIENTED_EDGE('',*,*,#9345,.T.);
#13170=ORIENTED_EDGE('',*,*,#9350,.T.);
#13171=ORIENTED_EDGE('',*,*,#9351,.F.);
#13172=ORIENTED_EDGE('',*,*,#9350,.F.);
#13173=ORIENTED_EDGE('',*,*,#9344,.F.);
#13174=ORIENTED_EDGE('',*,*,#9352,.F.);
#13175=ORIENTED_EDGE('',*,*,#9353,.T.);
#13176=ORIENTED_EDGE('',*,*,#9354,.F.);
#13177=ORIENTED_EDGE('',*,*,#9355,.F.);
#13178=ORIENTED_EDGE('',*,*,#9356,.F.);
#13179=ORIENTED_EDGE('',*,*,#9355,.T.);
#13180=ORIENTED_EDGE('',*,*,#9357,.T.);
#13181=ORIENTED_EDGE('',*,*,#9358,.F.);
#13182=ORIENTED_EDGE('',*,*,#9357,.F.);
#13183=ORIENTED_EDGE('',*,*,#9354,.T.);
#13184=ORIENTED_EDGE('',*,*,#9359,.T.);
#13185=ORIENTED_EDGE('',*,*,#9360,.F.);
#13186=ORIENTED_EDGE('',*,*,#9359,.F.);
#13187=ORIENTED_EDGE('',*,*,#9353,.F.);
#13188=ORIENTED_EDGE('',*,*,#9361,.F.);
#13189=ORIENTED_EDGE('',*,*,#9362,.T.);
#13190=ORIENTED_EDGE('',*,*,#9363,.F.);
#13191=ORIENTED_EDGE('',*,*,#9364,.F.);
#13192=ORIENTED_EDGE('',*,*,#9365,.F.);
#13193=ORIENTED_EDGE('',*,*,#9364,.T.);
#13194=ORIENTED_EDGE('',*,*,#9366,.T.);
#13195=ORIENTED_EDGE('',*,*,#9367,.F.);
#13196=ORIENTED_EDGE('',*,*,#9366,.F.);
#13197=ORIENTED_EDGE('',*,*,#9363,.T.);
#13198=ORIENTED_EDGE('',*,*,#9368,.T.);
#13199=ORIENTED_EDGE('',*,*,#9369,.F.);
#13200=ORIENTED_EDGE('',*,*,#9368,.F.);
#13201=ORIENTED_EDGE('',*,*,#9362,.F.);
#13202=ORIENTED_EDGE('',*,*,#9370,.F.);
#13203=ORIENTED_EDGE('',*,*,#9371,.T.);
#13204=ORIENTED_EDGE('',*,*,#9372,.F.);
#13205=ORIENTED_EDGE('',*,*,#9373,.F.);
#13206=ORIENTED_EDGE('',*,*,#9374,.F.);
#13207=ORIENTED_EDGE('',*,*,#9373,.T.);
#13208=ORIENTED_EDGE('',*,*,#9375,.T.);
#13209=ORIENTED_EDGE('',*,*,#9376,.F.);
#13210=ORIENTED_EDGE('',*,*,#9375,.F.);
#13211=ORIENTED_EDGE('',*,*,#9372,.T.);
#13212=ORIENTED_EDGE('',*,*,#9377,.T.);
#13213=ORIENTED_EDGE('',*,*,#9378,.F.);
#13214=ORIENTED_EDGE('',*,*,#9377,.F.);
#13215=ORIENTED_EDGE('',*,*,#9371,.F.);
#13216=ORIENTED_EDGE('',*,*,#9379,.F.);
#13217=ORIENTED_EDGE('',*,*,#9380,.T.);
#13218=ORIENTED_EDGE('',*,*,#9381,.F.);
#13219=ORIENTED_EDGE('',*,*,#9382,.F.);
#13220=ORIENTED_EDGE('',*,*,#9383,.F.);
#13221=ORIENTED_EDGE('',*,*,#9382,.T.);
#13222=ORIENTED_EDGE('',*,*,#9384,.T.);
#13223=ORIENTED_EDGE('',*,*,#9385,.F.);
#13224=ORIENTED_EDGE('',*,*,#9384,.F.);
#13225=ORIENTED_EDGE('',*,*,#9381,.T.);
#13226=ORIENTED_EDGE('',*,*,#9386,.T.);
#13227=ORIENTED_EDGE('',*,*,#9387,.F.);
#13228=ORIENTED_EDGE('',*,*,#9386,.F.);
#13229=ORIENTED_EDGE('',*,*,#9380,.F.);
#13230=ORIENTED_EDGE('',*,*,#9388,.F.);
#13231=ORIENTED_EDGE('',*,*,#9389,.T.);
#13232=ORIENTED_EDGE('',*,*,#9390,.F.);
#13233=ORIENTED_EDGE('',*,*,#9391,.F.);
#13234=ORIENTED_EDGE('',*,*,#9392,.F.);
#13235=ORIENTED_EDGE('',*,*,#9391,.T.);
#13236=ORIENTED_EDGE('',*,*,#9393,.T.);
#13237=ORIENTED_EDGE('',*,*,#9394,.F.);
#13238=ORIENTED_EDGE('',*,*,#9393,.F.);
#13239=ORIENTED_EDGE('',*,*,#9390,.T.);
#13240=ORIENTED_EDGE('',*,*,#9395,.T.);
#13241=ORIENTED_EDGE('',*,*,#9396,.F.);
#13242=ORIENTED_EDGE('',*,*,#9395,.F.);
#13243=ORIENTED_EDGE('',*,*,#9389,.F.);
#13244=ORIENTED_EDGE('',*,*,#9397,.F.);
#13245=ORIENTED_EDGE('',*,*,#9398,.T.);
#13246=ORIENTED_EDGE('',*,*,#9399,.F.);
#13247=ORIENTED_EDGE('',*,*,#9400,.F.);
#13248=ORIENTED_EDGE('',*,*,#9401,.F.);
#13249=ORIENTED_EDGE('',*,*,#9400,.T.);
#13250=ORIENTED_EDGE('',*,*,#9402,.T.);
#13251=ORIENTED_EDGE('',*,*,#9403,.F.);
#13252=ORIENTED_EDGE('',*,*,#9402,.F.);
#13253=ORIENTED_EDGE('',*,*,#9399,.T.);
#13254=ORIENTED_EDGE('',*,*,#9404,.T.);
#13255=ORIENTED_EDGE('',*,*,#9405,.F.);
#13256=ORIENTED_EDGE('',*,*,#9404,.F.);
#13257=ORIENTED_EDGE('',*,*,#9398,.F.);
#13258=ORIENTED_EDGE('',*,*,#9406,.F.);
#13259=ORIENTED_EDGE('',*,*,#9407,.T.);
#13260=ORIENTED_EDGE('',*,*,#9408,.F.);
#13261=ORIENTED_EDGE('',*,*,#9409,.F.);
#13262=ORIENTED_EDGE('',*,*,#9410,.F.);
#13263=ORIENTED_EDGE('',*,*,#9409,.T.);
#13264=ORIENTED_EDGE('',*,*,#9411,.T.);
#13265=ORIENTED_EDGE('',*,*,#9412,.F.);
#13266=ORIENTED_EDGE('',*,*,#9411,.F.);
#13267=ORIENTED_EDGE('',*,*,#9408,.T.);
#13268=ORIENTED_EDGE('',*,*,#9413,.T.);
#13269=ORIENTED_EDGE('',*,*,#9414,.F.);
#13270=ORIENTED_EDGE('',*,*,#9413,.F.);
#13271=ORIENTED_EDGE('',*,*,#9407,.F.);
#13272=ORIENTED_EDGE('',*,*,#9415,.F.);
#13273=ORIENTED_EDGE('',*,*,#9416,.T.);
#13274=ORIENTED_EDGE('',*,*,#9417,.F.);
#13275=ORIENTED_EDGE('',*,*,#9418,.F.);
#13276=ORIENTED_EDGE('',*,*,#9419,.F.);
#13277=ORIENTED_EDGE('',*,*,#9418,.T.);
#13278=ORIENTED_EDGE('',*,*,#9420,.T.);
#13279=ORIENTED_EDGE('',*,*,#9421,.F.);
#13280=ORIENTED_EDGE('',*,*,#9420,.F.);
#13281=ORIENTED_EDGE('',*,*,#9417,.T.);
#13282=ORIENTED_EDGE('',*,*,#9422,.T.);
#13283=ORIENTED_EDGE('',*,*,#9423,.F.);
#13284=ORIENTED_EDGE('',*,*,#9422,.F.);
#13285=ORIENTED_EDGE('',*,*,#9416,.F.);
#13286=ORIENTED_EDGE('',*,*,#9424,.F.);
#13287=ORIENTED_EDGE('',*,*,#9425,.T.);
#13288=ORIENTED_EDGE('',*,*,#9426,.F.);
#13289=ORIENTED_EDGE('',*,*,#9427,.F.);
#13290=ORIENTED_EDGE('',*,*,#9428,.F.);
#13291=ORIENTED_EDGE('',*,*,#9427,.T.);
#13292=ORIENTED_EDGE('',*,*,#9429,.T.);
#13293=ORIENTED_EDGE('',*,*,#9430,.F.);
#13294=ORIENTED_EDGE('',*,*,#9429,.F.);
#13295=ORIENTED_EDGE('',*,*,#9426,.T.);
#13296=ORIENTED_EDGE('',*,*,#9431,.T.);
#13297=ORIENTED_EDGE('',*,*,#9432,.F.);
#13298=ORIENTED_EDGE('',*,*,#9431,.F.);
#13299=ORIENTED_EDGE('',*,*,#9425,.F.);
#13300=ORIENTED_EDGE('',*,*,#9433,.F.);
#13301=ORIENTED_EDGE('',*,*,#9434,.T.);
#13302=ORIENTED_EDGE('',*,*,#9435,.F.);
#13303=ORIENTED_EDGE('',*,*,#9436,.F.);
#13304=ORIENTED_EDGE('',*,*,#9437,.F.);
#13305=ORIENTED_EDGE('',*,*,#9436,.T.);
#13306=ORIENTED_EDGE('',*,*,#9438,.T.);
#13307=ORIENTED_EDGE('',*,*,#9439,.F.);
#13308=ORIENTED_EDGE('',*,*,#9438,.F.);
#13309=ORIENTED_EDGE('',*,*,#9435,.T.);
#13310=ORIENTED_EDGE('',*,*,#9440,.T.);
#13311=ORIENTED_EDGE('',*,*,#9441,.F.);
#13312=ORIENTED_EDGE('',*,*,#9440,.F.);
#13313=ORIENTED_EDGE('',*,*,#9434,.F.);
#13314=ORIENTED_EDGE('',*,*,#9442,.F.);
#13315=ORIENTED_EDGE('',*,*,#9443,.T.);
#13316=ORIENTED_EDGE('',*,*,#9444,.F.);
#13317=ORIENTED_EDGE('',*,*,#9445,.F.);
#13318=ORIENTED_EDGE('',*,*,#9446,.F.);
#13319=ORIENTED_EDGE('',*,*,#9445,.T.);
#13320=ORIENTED_EDGE('',*,*,#9447,.T.);
#13321=ORIENTED_EDGE('',*,*,#9448,.F.);
#13322=ORIENTED_EDGE('',*,*,#9447,.F.);
#13323=ORIENTED_EDGE('',*,*,#9444,.T.);
#13324=ORIENTED_EDGE('',*,*,#9449,.T.);
#13325=ORIENTED_EDGE('',*,*,#9450,.F.);
#13326=ORIENTED_EDGE('',*,*,#9449,.F.);
#13327=ORIENTED_EDGE('',*,*,#9443,.F.);
#13328=ORIENTED_EDGE('',*,*,#9451,.F.);
#13329=ORIENTED_EDGE('',*,*,#9452,.T.);
#13330=ORIENTED_EDGE('',*,*,#9453,.F.);
#13331=ORIENTED_EDGE('',*,*,#9454,.F.);
#13332=ORIENTED_EDGE('',*,*,#9455,.F.);
#13333=ORIENTED_EDGE('',*,*,#9454,.T.);
#13334=ORIENTED_EDGE('',*,*,#9456,.T.);
#13335=ORIENTED_EDGE('',*,*,#9457,.F.);
#13336=ORIENTED_EDGE('',*,*,#9458,.F.);
#13337=ORIENTED_EDGE('',*,*,#9456,.F.);
#13338=ORIENTED_EDGE('',*,*,#9453,.T.);
#13339=ORIENTED_EDGE('',*,*,#9459,.T.);
#13340=ORIENTED_EDGE('',*,*,#9460,.F.);
#13341=ORIENTED_EDGE('',*,*,#9459,.F.);
#13342=ORIENTED_EDGE('',*,*,#9452,.F.);
#13343=ORIENTED_EDGE('',*,*,#9461,.F.);
#13344=ORIENTED_EDGE('',*,*,#9462,.F.);
#13345=ORIENTED_EDGE('',*,*,#9463,.T.);
#13346=ORIENTED_EDGE('',*,*,#9464,.F.);
#13347=ORIENTED_EDGE('',*,*,#9465,.F.);
#13348=ORIENTED_EDGE('',*,*,#9466,.F.);
#13349=ORIENTED_EDGE('',*,*,#9465,.T.);
#13350=ORIENTED_EDGE('',*,*,#9467,.T.);
#13351=ORIENTED_EDGE('',*,*,#9468,.F.);
#13352=ORIENTED_EDGE('',*,*,#9467,.F.);
#13353=ORIENTED_EDGE('',*,*,#9464,.T.);
#13354=ORIENTED_EDGE('',*,*,#9469,.T.);
#13355=ORIENTED_EDGE('',*,*,#9470,.F.);
#13356=ORIENTED_EDGE('',*,*,#9469,.F.);
#13357=ORIENTED_EDGE('',*,*,#9463,.F.);
#13358=ORIENTED_EDGE('',*,*,#9471,.F.);
#13359=ORIENTED_EDGE('',*,*,#9472,.T.);
#13360=ORIENTED_EDGE('',*,*,#9473,.F.);
#13361=ORIENTED_EDGE('',*,*,#9474,.F.);
#13362=ORIENTED_EDGE('',*,*,#9475,.F.);
#13363=ORIENTED_EDGE('',*,*,#9474,.T.);
#13364=ORIENTED_EDGE('',*,*,#9476,.T.);
#13365=ORIENTED_EDGE('',*,*,#9477,.F.);
#13366=ORIENTED_EDGE('',*,*,#9476,.F.);
#13367=ORIENTED_EDGE('',*,*,#9473,.T.);
#13368=ORIENTED_EDGE('',*,*,#9478,.T.);
#13369=ORIENTED_EDGE('',*,*,#9479,.F.);
#13370=ORIENTED_EDGE('',*,*,#9478,.F.);
#13371=ORIENTED_EDGE('',*,*,#9472,.F.);
#13372=ORIENTED_EDGE('',*,*,#9480,.F.);
#13373=ORIENTED_EDGE('',*,*,#9481,.T.);
#13374=ORIENTED_EDGE('',*,*,#9482,.F.);
#13375=ORIENTED_EDGE('',*,*,#9483,.F.);
#13376=ORIENTED_EDGE('',*,*,#9484,.F.);
#13377=ORIENTED_EDGE('',*,*,#9483,.T.);
#13378=ORIENTED_EDGE('',*,*,#9485,.T.);
#13379=ORIENTED_EDGE('',*,*,#9486,.F.);
#13380=ORIENTED_EDGE('',*,*,#9485,.F.);
#13381=ORIENTED_EDGE('',*,*,#9482,.T.);
#13382=ORIENTED_EDGE('',*,*,#9487,.T.);
#13383=ORIENTED_EDGE('',*,*,#9488,.F.);
#13384=ORIENTED_EDGE('',*,*,#9487,.F.);
#13385=ORIENTED_EDGE('',*,*,#9481,.F.);
#13386=ORIENTED_EDGE('',*,*,#9489,.F.);
#13387=ORIENTED_EDGE('',*,*,#9490,.T.);
#13388=ORIENTED_EDGE('',*,*,#9491,.F.);
#13389=ORIENTED_EDGE('',*,*,#9492,.F.);
#13390=ORIENTED_EDGE('',*,*,#9493,.F.);
#13391=ORIENTED_EDGE('',*,*,#9492,.T.);
#13392=ORIENTED_EDGE('',*,*,#9494,.T.);
#13393=ORIENTED_EDGE('',*,*,#9495,.F.);
#13394=ORIENTED_EDGE('',*,*,#9494,.F.);
#13395=ORIENTED_EDGE('',*,*,#9491,.T.);
#13396=ORIENTED_EDGE('',*,*,#9496,.T.);
#13397=ORIENTED_EDGE('',*,*,#9497,.F.);
#13398=ORIENTED_EDGE('',*,*,#9496,.F.);
#13399=ORIENTED_EDGE('',*,*,#9490,.F.);
#13400=ORIENTED_EDGE('',*,*,#9498,.F.);
#13401=ORIENTED_EDGE('',*,*,#9499,.T.);
#13402=ORIENTED_EDGE('',*,*,#9500,.F.);
#13403=ORIENTED_EDGE('',*,*,#9501,.F.);
#13404=ORIENTED_EDGE('',*,*,#9502,.F.);
#13405=ORIENTED_EDGE('',*,*,#9501,.T.);
#13406=ORIENTED_EDGE('',*,*,#9503,.T.);
#13407=ORIENTED_EDGE('',*,*,#9504,.F.);
#13408=ORIENTED_EDGE('',*,*,#9503,.F.);
#13409=ORIENTED_EDGE('',*,*,#9500,.T.);
#13410=ORIENTED_EDGE('',*,*,#9505,.T.);
#13411=ORIENTED_EDGE('',*,*,#9506,.F.);
#13412=ORIENTED_EDGE('',*,*,#9505,.F.);
#13413=ORIENTED_EDGE('',*,*,#9499,.F.);
#13414=ORIENTED_EDGE('',*,*,#9507,.F.);
#13415=ORIENTED_EDGE('',*,*,#9508,.T.);
#13416=ORIENTED_EDGE('',*,*,#9509,.F.);
#13417=ORIENTED_EDGE('',*,*,#9510,.F.);
#13418=ORIENTED_EDGE('',*,*,#9511,.F.);
#13419=ORIENTED_EDGE('',*,*,#9510,.T.);
#13420=ORIENTED_EDGE('',*,*,#9512,.T.);
#13421=ORIENTED_EDGE('',*,*,#9513,.F.);
#13422=ORIENTED_EDGE('',*,*,#9512,.F.);
#13423=ORIENTED_EDGE('',*,*,#9509,.T.);
#13424=ORIENTED_EDGE('',*,*,#9514,.T.);
#13425=ORIENTED_EDGE('',*,*,#9515,.F.);
#13426=ORIENTED_EDGE('',*,*,#9514,.F.);
#13427=ORIENTED_EDGE('',*,*,#9508,.F.);
#13428=ORIENTED_EDGE('',*,*,#9516,.F.);
#13429=ORIENTED_EDGE('',*,*,#9517,.T.);
#13430=ORIENTED_EDGE('',*,*,#9518,.F.);
#13431=ORIENTED_EDGE('',*,*,#9519,.F.);
#13432=ORIENTED_EDGE('',*,*,#9520,.F.);
#13433=ORIENTED_EDGE('',*,*,#9519,.T.);
#13434=ORIENTED_EDGE('',*,*,#9521,.T.);
#13435=ORIENTED_EDGE('',*,*,#9522,.F.);
#13436=ORIENTED_EDGE('',*,*,#9521,.F.);
#13437=ORIENTED_EDGE('',*,*,#9518,.T.);
#13438=ORIENTED_EDGE('',*,*,#9523,.T.);
#13439=ORIENTED_EDGE('',*,*,#9524,.F.);
#13440=ORIENTED_EDGE('',*,*,#9523,.F.);
#13441=ORIENTED_EDGE('',*,*,#9517,.F.);
#13442=ORIENTED_EDGE('',*,*,#9525,.F.);
#13443=ORIENTED_EDGE('',*,*,#9526,.T.);
#13444=ORIENTED_EDGE('',*,*,#9527,.F.);
#13445=ORIENTED_EDGE('',*,*,#9528,.F.);
#13446=ORIENTED_EDGE('',*,*,#9529,.F.);
#13447=ORIENTED_EDGE('',*,*,#9528,.T.);
#13448=ORIENTED_EDGE('',*,*,#9530,.T.);
#13449=ORIENTED_EDGE('',*,*,#9531,.F.);
#13450=ORIENTED_EDGE('',*,*,#9530,.F.);
#13451=ORIENTED_EDGE('',*,*,#9527,.T.);
#13452=ORIENTED_EDGE('',*,*,#9532,.T.);
#13453=ORIENTED_EDGE('',*,*,#9533,.F.);
#13454=ORIENTED_EDGE('',*,*,#9532,.F.);
#13455=ORIENTED_EDGE('',*,*,#9526,.F.);
#13456=ORIENTED_EDGE('',*,*,#9534,.F.);
#13457=ORIENTED_EDGE('',*,*,#9535,.T.);
#13458=ORIENTED_EDGE('',*,*,#9536,.F.);
#13459=ORIENTED_EDGE('',*,*,#9537,.F.);
#13460=ORIENTED_EDGE('',*,*,#9538,.F.);
#13461=ORIENTED_EDGE('',*,*,#9537,.T.);
#13462=ORIENTED_EDGE('',*,*,#9539,.T.);
#13463=ORIENTED_EDGE('',*,*,#9540,.F.);
#13464=ORIENTED_EDGE('',*,*,#9539,.F.);
#13465=ORIENTED_EDGE('',*,*,#9536,.T.);
#13466=ORIENTED_EDGE('',*,*,#9541,.T.);
#13467=ORIENTED_EDGE('',*,*,#9542,.F.);
#13468=ORIENTED_EDGE('',*,*,#9541,.F.);
#13469=ORIENTED_EDGE('',*,*,#9535,.F.);
#13470=ORIENTED_EDGE('',*,*,#9543,.F.);
#13471=ORIENTED_EDGE('',*,*,#9544,.T.);
#13472=ORIENTED_EDGE('',*,*,#9545,.F.);
#13473=ORIENTED_EDGE('',*,*,#9546,.F.);
#13474=ORIENTED_EDGE('',*,*,#9547,.F.);
#13475=ORIENTED_EDGE('',*,*,#9546,.T.);
#13476=ORIENTED_EDGE('',*,*,#9548,.T.);
#13477=ORIENTED_EDGE('',*,*,#9549,.F.);
#13478=ORIENTED_EDGE('',*,*,#9548,.F.);
#13479=ORIENTED_EDGE('',*,*,#9545,.T.);
#13480=ORIENTED_EDGE('',*,*,#9550,.T.);
#13481=ORIENTED_EDGE('',*,*,#9551,.F.);
#13482=ORIENTED_EDGE('',*,*,#9550,.F.);
#13483=ORIENTED_EDGE('',*,*,#9544,.F.);
#13484=ORIENTED_EDGE('',*,*,#9552,.F.);
#13485=ORIENTED_EDGE('',*,*,#9553,.T.);
#13486=ORIENTED_EDGE('',*,*,#9554,.F.);
#13487=ORIENTED_EDGE('',*,*,#9555,.F.);
#13488=ORIENTED_EDGE('',*,*,#9556,.F.);
#13489=ORIENTED_EDGE('',*,*,#9555,.T.);
#13490=ORIENTED_EDGE('',*,*,#9557,.T.);
#13491=ORIENTED_EDGE('',*,*,#9558,.F.);
#13492=ORIENTED_EDGE('',*,*,#9557,.F.);
#13493=ORIENTED_EDGE('',*,*,#9554,.T.);
#13494=ORIENTED_EDGE('',*,*,#9559,.T.);
#13495=ORIENTED_EDGE('',*,*,#9560,.F.);
#13496=ORIENTED_EDGE('',*,*,#9559,.F.);
#13497=ORIENTED_EDGE('',*,*,#9553,.F.);
#13498=ORIENTED_EDGE('',*,*,#9561,.F.);
#13499=ORIENTED_EDGE('',*,*,#9562,.T.);
#13500=ORIENTED_EDGE('',*,*,#9563,.F.);
#13501=ORIENTED_EDGE('',*,*,#9564,.F.);
#13502=ORIENTED_EDGE('',*,*,#9565,.F.);
#13503=ORIENTED_EDGE('',*,*,#9564,.T.);
#13504=ORIENTED_EDGE('',*,*,#9566,.T.);
#13505=ORIENTED_EDGE('',*,*,#9567,.F.);
#13506=ORIENTED_EDGE('',*,*,#9566,.F.);
#13507=ORIENTED_EDGE('',*,*,#9563,.T.);
#13508=ORIENTED_EDGE('',*,*,#9568,.T.);
#13509=ORIENTED_EDGE('',*,*,#9569,.F.);
#13510=ORIENTED_EDGE('',*,*,#9568,.F.);
#13511=ORIENTED_EDGE('',*,*,#9562,.F.);
#13512=ORIENTED_EDGE('',*,*,#9570,.F.);
#13513=ORIENTED_EDGE('',*,*,#9571,.T.);
#13514=ORIENTED_EDGE('',*,*,#9572,.F.);
#13515=ORIENTED_EDGE('',*,*,#9573,.F.);
#13516=ORIENTED_EDGE('',*,*,#9574,.F.);
#13517=ORIENTED_EDGE('',*,*,#9573,.T.);
#13518=ORIENTED_EDGE('',*,*,#9575,.T.);
#13519=ORIENTED_EDGE('',*,*,#9576,.F.);
#13520=ORIENTED_EDGE('',*,*,#9575,.F.);
#13521=ORIENTED_EDGE('',*,*,#9572,.T.);
#13522=ORIENTED_EDGE('',*,*,#9577,.T.);
#13523=ORIENTED_EDGE('',*,*,#9578,.F.);
#13524=ORIENTED_EDGE('',*,*,#9577,.F.);
#13525=ORIENTED_EDGE('',*,*,#9571,.F.);
#13526=ORIENTED_EDGE('',*,*,#9579,.F.);
#13527=ORIENTED_EDGE('',*,*,#9580,.T.);
#13528=ORIENTED_EDGE('',*,*,#9581,.F.);
#13529=ORIENTED_EDGE('',*,*,#9582,.F.);
#13530=ORIENTED_EDGE('',*,*,#9583,.F.);
#13531=ORIENTED_EDGE('',*,*,#9582,.T.);
#13532=ORIENTED_EDGE('',*,*,#9584,.T.);
#13533=ORIENTED_EDGE('',*,*,#9585,.F.);
#13534=ORIENTED_EDGE('',*,*,#9584,.F.);
#13535=ORIENTED_EDGE('',*,*,#9581,.T.);
#13536=ORIENTED_EDGE('',*,*,#9586,.T.);
#13537=ORIENTED_EDGE('',*,*,#9587,.F.);
#13538=ORIENTED_EDGE('',*,*,#9586,.F.);
#13539=ORIENTED_EDGE('',*,*,#9580,.F.);
#13540=ORIENTED_EDGE('',*,*,#9588,.F.);
#13541=ORIENTED_EDGE('',*,*,#9589,.T.);
#13542=ORIENTED_EDGE('',*,*,#9590,.F.);
#13543=ORIENTED_EDGE('',*,*,#9591,.F.);
#13544=ORIENTED_EDGE('',*,*,#9592,.F.);
#13545=ORIENTED_EDGE('',*,*,#9591,.T.);
#13546=ORIENTED_EDGE('',*,*,#9593,.T.);
#13547=ORIENTED_EDGE('',*,*,#9594,.F.);
#13548=ORIENTED_EDGE('',*,*,#9593,.F.);
#13549=ORIENTED_EDGE('',*,*,#9590,.T.);
#13550=ORIENTED_EDGE('',*,*,#9595,.T.);
#13551=ORIENTED_EDGE('',*,*,#9596,.F.);
#13552=ORIENTED_EDGE('',*,*,#9595,.F.);
#13553=ORIENTED_EDGE('',*,*,#9589,.F.);
#13554=ORIENTED_EDGE('',*,*,#9597,.F.);
#13555=ORIENTED_EDGE('',*,*,#9598,.T.);
#13556=ORIENTED_EDGE('',*,*,#9599,.F.);
#13557=ORIENTED_EDGE('',*,*,#9600,.F.);
#13558=ORIENTED_EDGE('',*,*,#9601,.F.);
#13559=ORIENTED_EDGE('',*,*,#9600,.T.);
#13560=ORIENTED_EDGE('',*,*,#9602,.T.);
#13561=ORIENTED_EDGE('',*,*,#9603,.F.);
#13562=ORIENTED_EDGE('',*,*,#9602,.F.);
#13563=ORIENTED_EDGE('',*,*,#9599,.T.);
#13564=ORIENTED_EDGE('',*,*,#9604,.T.);
#13565=ORIENTED_EDGE('',*,*,#9605,.F.);
#13566=ORIENTED_EDGE('',*,*,#9604,.F.);
#13567=ORIENTED_EDGE('',*,*,#9598,.F.);
#13568=ORIENTED_EDGE('',*,*,#9606,.F.);
#13569=ORIENTED_EDGE('',*,*,#9607,.T.);
#13570=ORIENTED_EDGE('',*,*,#9608,.F.);
#13571=ORIENTED_EDGE('',*,*,#9609,.F.);
#13572=ORIENTED_EDGE('',*,*,#9610,.F.);
#13573=ORIENTED_EDGE('',*,*,#9609,.T.);
#13574=ORIENTED_EDGE('',*,*,#9611,.T.);
#13575=ORIENTED_EDGE('',*,*,#9612,.F.);
#13576=ORIENTED_EDGE('',*,*,#9611,.F.);
#13577=ORIENTED_EDGE('',*,*,#9608,.T.);
#13578=ORIENTED_EDGE('',*,*,#9613,.T.);
#13579=ORIENTED_EDGE('',*,*,#9614,.F.);
#13580=ORIENTED_EDGE('',*,*,#9613,.F.);
#13581=ORIENTED_EDGE('',*,*,#9607,.F.);
#13582=ORIENTED_EDGE('',*,*,#9615,.F.);
#13583=ORIENTED_EDGE('',*,*,#9616,.T.);
#13584=ORIENTED_EDGE('',*,*,#9617,.F.);
#13585=ORIENTED_EDGE('',*,*,#9618,.F.);
#13586=ORIENTED_EDGE('',*,*,#9619,.F.);
#13587=ORIENTED_EDGE('',*,*,#9618,.T.);
#13588=ORIENTED_EDGE('',*,*,#9620,.T.);
#13589=ORIENTED_EDGE('',*,*,#9621,.F.);
#13590=ORIENTED_EDGE('',*,*,#9620,.F.);
#13591=ORIENTED_EDGE('',*,*,#9617,.T.);
#13592=ORIENTED_EDGE('',*,*,#9622,.T.);
#13593=ORIENTED_EDGE('',*,*,#9623,.F.);
#13594=ORIENTED_EDGE('',*,*,#9622,.F.);
#13595=ORIENTED_EDGE('',*,*,#9616,.F.);
#13596=ORIENTED_EDGE('',*,*,#9624,.F.);
#13597=ORIENTED_EDGE('',*,*,#9625,.T.);
#13598=ORIENTED_EDGE('',*,*,#9626,.T.);
#13599=ORIENTED_EDGE('',*,*,#9627,.F.);
#13600=ORIENTED_EDGE('',*,*,#9628,.F.);
#13601=ORIENTED_EDGE('',*,*,#9629,.T.);
#13602=ORIENTED_EDGE('',*,*,#9630,.T.);
#13603=ORIENTED_EDGE('',*,*,#9625,.F.);
#13604=ORIENTED_EDGE('',*,*,#9631,.F.);
#13605=ORIENTED_EDGE('',*,*,#9632,.T.);
#13606=ORIENTED_EDGE('',*,*,#9633,.T.);
#13607=ORIENTED_EDGE('',*,*,#9629,.F.);
#13608=ORIENTED_EDGE('',*,*,#9634,.F.);
#13609=ORIENTED_EDGE('',*,*,#9635,.T.);
#13610=ORIENTED_EDGE('',*,*,#9636,.T.);
#13611=ORIENTED_EDGE('',*,*,#9632,.F.);
#13612=ORIENTED_EDGE('',*,*,#9637,.F.);
#13613=ORIENTED_EDGE('',*,*,#9638,.T.);
#13614=ORIENTED_EDGE('',*,*,#9639,.T.);
#13615=ORIENTED_EDGE('',*,*,#9635,.F.);
#13616=ORIENTED_EDGE('',*,*,#9640,.F.);
#13617=ORIENTED_EDGE('',*,*,#9627,.T.);
#13618=ORIENTED_EDGE('',*,*,#9641,.T.);
#13619=ORIENTED_EDGE('',*,*,#9638,.F.);
#13620=ORIENTED_EDGE('',*,*,#9641,.F.);
#13621=ORIENTED_EDGE('',*,*,#9626,.F.);
#13622=ORIENTED_EDGE('',*,*,#9630,.F.);
#13623=ORIENTED_EDGE('',*,*,#9633,.F.);
#13624=ORIENTED_EDGE('',*,*,#9636,.F.);
#13625=ORIENTED_EDGE('',*,*,#9639,.F.);
#13626=ORIENTED_EDGE('',*,*,#9642,.F.);
#13627=ORIENTED_EDGE('',*,*,#9291,.F.);
#13628=ORIENTED_EDGE('',*,*,#9083,.F.);
#13629=ORIENTED_EDGE('',*,*,#9292,.F.);
#13630=ORIENTED_EDGE('',*,*,#9643,.T.);
#13631=ORIENTED_EDGE('',*,*,#9642,.T.);
#13632=ORIENTED_EDGE('',*,*,#9643,.F.);
#13633=ORIENTED_EDGE('',*,*,#9181,.T.);
#13634=ORIENTED_EDGE('',*,*,#9288,.T.);
#13635=ORIENTED_EDGE('',*,*,#9644,.F.);
#13636=ORIENTED_EDGE('',*,*,#9297,.T.);
#13637=ORIENTED_EDGE('',*,*,#9645,.F.);
#13638=ORIENTED_EDGE('',*,*,#9644,.T.);
#13639=ORIENTED_EDGE('',*,*,#9287,.T.);
#13640=ORIENTED_EDGE('',*,*,#9186,.T.);
#13641=ORIENTED_EDGE('',*,*,#9296,.T.);
#13642=ORIENTED_EDGE('',*,*,#9646,.F.);
#13643=ORIENTED_EDGE('',*,*,#9647,.T.);
#13644=ORIENTED_EDGE('',*,*,#9461,.T.);
#13645=ORIENTED_EDGE('',*,*,#9451,.T.);
#13646=ORIENTED_EDGE('',*,*,#9455,.T.);
#13647=ORIENTED_EDGE('',*,*,#9648,.T.);
#13648=ORIENTED_EDGE('',*,*,#9645,.T.);
#13649=ORIENTED_EDGE('',*,*,#9648,.F.);
#13650=ORIENTED_EDGE('',*,*,#9457,.T.);
#13651=ORIENTED_EDGE('',*,*,#9458,.T.);
#13652=ORIENTED_EDGE('',*,*,#9460,.T.);
#13653=ORIENTED_EDGE('',*,*,#9647,.F.);
#13654=ORIENTED_EDGE('',*,*,#9304,.T.);
#13655=ORIENTED_EDGE('',*,*,#9306,.T.);
#13656=ORIENTED_EDGE('',*,*,#9298,.T.);
#13657=ORIENTED_EDGE('',*,*,#9302,.T.);
#13658=ORIENTED_EDGE('',*,*,#9313,.T.);
#13659=ORIENTED_EDGE('',*,*,#9315,.T.);
#13660=ORIENTED_EDGE('',*,*,#9307,.T.);
#13661=ORIENTED_EDGE('',*,*,#9311,.T.);
#13662=ORIENTED_EDGE('',*,*,#9322,.T.);
#13663=ORIENTED_EDGE('',*,*,#9324,.T.);
#13664=ORIENTED_EDGE('',*,*,#9316,.T.);
#13665=ORIENTED_EDGE('',*,*,#9320,.T.);
#13666=ORIENTED_EDGE('',*,*,#9331,.T.);
#13667=ORIENTED_EDGE('',*,*,#9333,.T.);
#13668=ORIENTED_EDGE('',*,*,#9325,.T.);
#13669=ORIENTED_EDGE('',*,*,#9329,.T.);
#13670=ORIENTED_EDGE('',*,*,#9340,.T.);
#13671=ORIENTED_EDGE('',*,*,#9342,.T.);
#13672=ORIENTED_EDGE('',*,*,#9334,.T.);
#13673=ORIENTED_EDGE('',*,*,#9338,.T.);
#13674=ORIENTED_EDGE('',*,*,#9349,.T.);
#13675=ORIENTED_EDGE('',*,*,#9351,.T.);
#13676=ORIENTED_EDGE('',*,*,#9343,.T.);
#13677=ORIENTED_EDGE('',*,*,#9347,.T.);
#13678=ORIENTED_EDGE('',*,*,#9358,.T.);
#13679=ORIENTED_EDGE('',*,*,#9360,.T.);
#13680=ORIENTED_EDGE('',*,*,#9352,.T.);
#13681=ORIENTED_EDGE('',*,*,#9356,.T.);
#13682=ORIENTED_EDGE('',*,*,#9367,.T.);
#13683=ORIENTED_EDGE('',*,*,#9369,.T.);
#13684=ORIENTED_EDGE('',*,*,#9361,.T.);
#13685=ORIENTED_EDGE('',*,*,#9365,.T.);
#13686=ORIENTED_EDGE('',*,*,#9376,.T.);
#13687=ORIENTED_EDGE('',*,*,#9378,.T.);
#13688=ORIENTED_EDGE('',*,*,#9370,.T.);
#13689=ORIENTED_EDGE('',*,*,#9374,.T.);
#13690=ORIENTED_EDGE('',*,*,#9385,.T.);
#13691=ORIENTED_EDGE('',*,*,#9387,.T.);
#13692=ORIENTED_EDGE('',*,*,#9379,.T.);
#13693=ORIENTED_EDGE('',*,*,#9383,.T.);
#13694=ORIENTED_EDGE('',*,*,#9394,.T.);
#13695=ORIENTED_EDGE('',*,*,#9396,.T.);
#13696=ORIENTED_EDGE('',*,*,#9388,.T.);
#13697=ORIENTED_EDGE('',*,*,#9392,.T.);
#13698=ORIENTED_EDGE('',*,*,#9403,.T.);
#13699=ORIENTED_EDGE('',*,*,#9405,.T.);
#13700=ORIENTED_EDGE('',*,*,#9397,.T.);
#13701=ORIENTED_EDGE('',*,*,#9401,.T.);
#13702=ORIENTED_EDGE('',*,*,#9412,.T.);
#13703=ORIENTED_EDGE('',*,*,#9414,.T.);
#13704=ORIENTED_EDGE('',*,*,#9406,.T.);
#13705=ORIENTED_EDGE('',*,*,#9410,.T.);
#13706=ORIENTED_EDGE('',*,*,#9421,.T.);
#13707=ORIENTED_EDGE('',*,*,#9423,.T.);
#13708=ORIENTED_EDGE('',*,*,#9415,.T.);
#13709=ORIENTED_EDGE('',*,*,#9419,.T.);
#13710=ORIENTED_EDGE('',*,*,#9430,.T.);
#13711=ORIENTED_EDGE('',*,*,#9432,.T.);
#13712=ORIENTED_EDGE('',*,*,#9424,.T.);
#13713=ORIENTED_EDGE('',*,*,#9428,.T.);
#13714=ORIENTED_EDGE('',*,*,#9439,.T.);
#13715=ORIENTED_EDGE('',*,*,#9441,.T.);
#13716=ORIENTED_EDGE('',*,*,#9433,.T.);
#13717=ORIENTED_EDGE('',*,*,#9437,.T.);
#13718=ORIENTED_EDGE('',*,*,#9448,.T.);
#13719=ORIENTED_EDGE('',*,*,#9450,.T.);
#13720=ORIENTED_EDGE('',*,*,#9442,.T.);
#13721=ORIENTED_EDGE('',*,*,#9446,.T.);
#13722=ORIENTED_EDGE('',*,*,#9468,.T.);
#13723=ORIENTED_EDGE('',*,*,#9470,.T.);
#13724=ORIENTED_EDGE('',*,*,#9462,.T.);
#13725=ORIENTED_EDGE('',*,*,#9466,.T.);
#13726=ORIENTED_EDGE('',*,*,#9477,.T.);
#13727=ORIENTED_EDGE('',*,*,#9479,.T.);
#13728=ORIENTED_EDGE('',*,*,#9471,.T.);
#13729=ORIENTED_EDGE('',*,*,#9475,.T.);
#13730=ORIENTED_EDGE('',*,*,#9486,.T.);
#13731=ORIENTED_EDGE('',*,*,#9488,.T.);
#13732=ORIENTED_EDGE('',*,*,#9480,.T.);
#13733=ORIENTED_EDGE('',*,*,#9484,.T.);
#13734=ORIENTED_EDGE('',*,*,#9495,.T.);
#13735=ORIENTED_EDGE('',*,*,#9497,.T.);
#13736=ORIENTED_EDGE('',*,*,#9489,.T.);
#13737=ORIENTED_EDGE('',*,*,#9493,.T.);
#13738=ORIENTED_EDGE('',*,*,#9504,.T.);
#13739=ORIENTED_EDGE('',*,*,#9506,.T.);
#13740=ORIENTED_EDGE('',*,*,#9498,.T.);
#13741=ORIENTED_EDGE('',*,*,#9502,.T.);
#13742=ORIENTED_EDGE('',*,*,#9513,.T.);
#13743=ORIENTED_EDGE('',*,*,#9515,.T.);
#13744=ORIENTED_EDGE('',*,*,#9507,.T.);
#13745=ORIENTED_EDGE('',*,*,#9511,.T.);
#13746=ORIENTED_EDGE('',*,*,#9522,.T.);
#13747=ORIENTED_EDGE('',*,*,#9524,.T.);
#13748=ORIENTED_EDGE('',*,*,#9516,.T.);
#13749=ORIENTED_EDGE('',*,*,#9520,.T.);
#13750=ORIENTED_EDGE('',*,*,#9531,.T.);
#13751=ORIENTED_EDGE('',*,*,#9533,.T.);
#13752=ORIENTED_EDGE('',*,*,#9525,.T.);
#13753=ORIENTED_EDGE('',*,*,#9529,.T.);
#13754=ORIENTED_EDGE('',*,*,#9540,.T.);
#13755=ORIENTED_EDGE('',*,*,#9542,.T.);
#13756=ORIENTED_EDGE('',*,*,#9534,.T.);
#13757=ORIENTED_EDGE('',*,*,#9538,.T.);
#13758=ORIENTED_EDGE('',*,*,#9549,.T.);
#13759=ORIENTED_EDGE('',*,*,#9551,.T.);
#13760=ORIENTED_EDGE('',*,*,#9543,.T.);
#13761=ORIENTED_EDGE('',*,*,#9547,.T.);
#13762=ORIENTED_EDGE('',*,*,#9558,.T.);
#13763=ORIENTED_EDGE('',*,*,#9560,.T.);
#13764=ORIENTED_EDGE('',*,*,#9552,.T.);
#13765=ORIENTED_EDGE('',*,*,#9556,.T.);
#13766=ORIENTED_EDGE('',*,*,#9567,.T.);
#13767=ORIENTED_EDGE('',*,*,#9569,.T.);
#13768=ORIENTED_EDGE('',*,*,#9561,.T.);
#13769=ORIENTED_EDGE('',*,*,#9565,.T.);
#13770=ORIENTED_EDGE('',*,*,#9576,.T.);
#13771=ORIENTED_EDGE('',*,*,#9578,.T.);
#13772=ORIENTED_EDGE('',*,*,#9570,.T.);
#13773=ORIENTED_EDGE('',*,*,#9574,.T.);
#13774=ORIENTED_EDGE('',*,*,#9585,.T.);
#13775=ORIENTED_EDGE('',*,*,#9587,.T.);
#13776=ORIENTED_EDGE('',*,*,#9579,.T.);
#13777=ORIENTED_EDGE('',*,*,#9583,.T.);
#13778=ORIENTED_EDGE('',*,*,#9594,.T.);
#13779=ORIENTED_EDGE('',*,*,#9596,.T.);
#13780=ORIENTED_EDGE('',*,*,#9588,.T.);
#13781=ORIENTED_EDGE('',*,*,#9592,.T.);
#13782=ORIENTED_EDGE('',*,*,#9603,.T.);
#13783=ORIENTED_EDGE('',*,*,#9605,.T.);
#13784=ORIENTED_EDGE('',*,*,#9597,.T.);
#13785=ORIENTED_EDGE('',*,*,#9601,.T.);
#13786=ORIENTED_EDGE('',*,*,#9612,.T.);
#13787=ORIENTED_EDGE('',*,*,#9614,.T.);
#13788=ORIENTED_EDGE('',*,*,#9606,.T.);
#13789=ORIENTED_EDGE('',*,*,#9610,.T.);
#13790=ORIENTED_EDGE('',*,*,#9621,.T.);
#13791=ORIENTED_EDGE('',*,*,#9623,.T.);
#13792=ORIENTED_EDGE('',*,*,#9615,.T.);
#13793=ORIENTED_EDGE('',*,*,#9619,.T.);
#13794=ORIENTED_EDGE('',*,*,#9649,.F.);
#13795=ORIENTED_EDGE('',*,*,#9650,.T.);
#13796=ORIENTED_EDGE('',*,*,#9646,.T.);
#13797=ORIENTED_EDGE('',*,*,#9650,.F.);
#13798=ORIENTED_EDGE('',*,*,#9649,.T.);
#13799=ORIENTED_EDGE('',*,*,#9624,.T.);
#13800=ORIENTED_EDGE('',*,*,#9640,.T.);
#13801=ORIENTED_EDGE('',*,*,#9637,.T.);
#13802=ORIENTED_EDGE('',*,*,#9634,.T.);
#13803=ORIENTED_EDGE('',*,*,#9631,.T.);
#13804=ORIENTED_EDGE('',*,*,#9628,.T.);
#13805=ORIENTED_EDGE('',*,*,#9651,.F.);
#13806=ORIENTED_EDGE('',*,*,#9652,.T.);
#13807=ORIENTED_EDGE('',*,*,#9653,.T.);
#13808=ORIENTED_EDGE('',*,*,#9654,.T.);
#13809=ORIENTED_EDGE('',*,*,#9655,.F.);
#13810=ORIENTED_EDGE('',*,*,#9656,.T.);
#13811=ORIENTED_EDGE('',*,*,#9651,.T.);
#13812=ORIENTED_EDGE('',*,*,#9657,.T.);
#13813=ORIENTED_EDGE('',*,*,#9658,.F.);
#13814=ORIENTED_EDGE('',*,*,#9659,.T.);
#13815=ORIENTED_EDGE('',*,*,#9655,.T.);
#13816=ORIENTED_EDGE('',*,*,#9660,.T.);
#13817=ORIENTED_EDGE('',*,*,#9661,.F.);
#13818=ORIENTED_EDGE('',*,*,#9662,.T.);
#13819=ORIENTED_EDGE('',*,*,#9658,.T.);
#13820=ORIENTED_EDGE('',*,*,#9663,.T.);
#13821=ORIENTED_EDGE('',*,*,#9664,.F.);
#13822=ORIENTED_EDGE('',*,*,#9665,.T.);
#13823=ORIENTED_EDGE('',*,*,#9661,.T.);
#13824=ORIENTED_EDGE('',*,*,#9666,.T.);
#13825=ORIENTED_EDGE('',*,*,#9667,.F.);
#13826=ORIENTED_EDGE('',*,*,#9668,.T.);
#13827=ORIENTED_EDGE('',*,*,#9664,.T.);
#13828=ORIENTED_EDGE('',*,*,#9669,.T.);
#13829=ORIENTED_EDGE('',*,*,#9670,.F.);
#13830=ORIENTED_EDGE('',*,*,#9671,.T.);
#13831=ORIENTED_EDGE('',*,*,#9667,.T.);
#13832=ORIENTED_EDGE('',*,*,#9672,.T.);
#13833=ORIENTED_EDGE('',*,*,#9673,.F.);
#13834=ORIENTED_EDGE('',*,*,#9674,.T.);
#13835=ORIENTED_EDGE('',*,*,#9675,.F.);
#13836=ORIENTED_EDGE('',*,*,#9676,.F.);
#13837=ORIENTED_EDGE('',*,*,#9677,.T.);
#13838=ORIENTED_EDGE('',*,*,#9673,.T.);
#13839=ORIENTED_EDGE('',*,*,#9678,.F.);
#13840=ORIENTED_EDGE('',*,*,#9679,.F.);
#13841=ORIENTED_EDGE('',*,*,#9680,.F.);
#13842=ORIENTED_EDGE('',*,*,#9681,.T.);
#13843=ORIENTED_EDGE('',*,*,#9676,.T.);
#13844=ORIENTED_EDGE('',*,*,#9682,.F.);
#13845=ORIENTED_EDGE('',*,*,#9683,.F.);
#13846=ORIENTED_EDGE('',*,*,#9684,.T.);
#13847=ORIENTED_EDGE('',*,*,#9680,.T.);
#13848=ORIENTED_EDGE('',*,*,#9685,.F.);
#13849=ORIENTED_EDGE('',*,*,#9686,.F.);
#13850=ORIENTED_EDGE('',*,*,#9687,.T.);
#13851=ORIENTED_EDGE('',*,*,#9683,.T.);
#13852=ORIENTED_EDGE('',*,*,#9688,.F.);
#13853=ORIENTED_EDGE('',*,*,#9689,.F.);
#13854=ORIENTED_EDGE('',*,*,#9690,.T.);
#13855=ORIENTED_EDGE('',*,*,#9686,.T.);
#13856=ORIENTED_EDGE('',*,*,#9691,.F.);
#13857=ORIENTED_EDGE('',*,*,#9692,.F.);
#13858=ORIENTED_EDGE('',*,*,#9693,.T.);
#13859=ORIENTED_EDGE('',*,*,#9689,.T.);
#13860=ORIENTED_EDGE('',*,*,#9694,.F.);
#13861=ORIENTED_EDGE('',*,*,#9695,.F.);
#13862=ORIENTED_EDGE('',*,*,#9696,.F.);
#13863=ORIENTED_EDGE('',*,*,#9697,.F.);
#13864=ORIENTED_EDGE('',*,*,#9698,.F.);
#13865=ORIENTED_EDGE('',*,*,#9699,.T.);
#13866=ORIENTED_EDGE('',*,*,#9696,.T.);
#13867=ORIENTED_EDGE('',*,*,#9700,.T.);
#13868=ORIENTED_EDGE('',*,*,#9701,.F.);
#13869=ORIENTED_EDGE('',*,*,#9702,.F.);
#13870=ORIENTED_EDGE('',*,*,#9703,.F.);
#13871=ORIENTED_EDGE('',*,*,#9704,.F.);
#13872=ORIENTED_EDGE('',*,*,#9705,.T.);
#13873=ORIENTED_EDGE('',*,*,#9702,.T.);
#13874=ORIENTED_EDGE('',*,*,#9706,.T.);
#13875=ORIENTED_EDGE('',*,*,#9695,.T.);
#13876=ORIENTED_EDGE('',*,*,#9707,.T.);
#13877=ORIENTED_EDGE('',*,*,#9703,.T.);
#13878=ORIENTED_EDGE('',*,*,#9708,.T.);
#13879=ORIENTED_EDGE('',*,*,#9709,.F.);
#13880=ORIENTED_EDGE('',*,*,#9710,.F.);
#13881=ORIENTED_EDGE('',*,*,#9711,.F.);
#13882=ORIENTED_EDGE('',*,*,#9712,.F.);
#13883=ORIENTED_EDGE('',*,*,#9713,.T.);
#13884=ORIENTED_EDGE('',*,*,#9710,.T.);
#13885=ORIENTED_EDGE('',*,*,#9714,.T.);
#13886=ORIENTED_EDGE('',*,*,#9715,.F.);
#13887=ORIENTED_EDGE('',*,*,#9716,.F.);
#13888=ORIENTED_EDGE('',*,*,#9717,.F.);
#13889=ORIENTED_EDGE('',*,*,#9718,.F.);
#13890=ORIENTED_EDGE('',*,*,#9719,.T.);
#13891=ORIENTED_EDGE('',*,*,#9716,.T.);
#13892=ORIENTED_EDGE('',*,*,#9720,.T.);
#13893=ORIENTED_EDGE('',*,*,#9701,.T.);
#13894=ORIENTED_EDGE('',*,*,#9721,.T.);
#13895=ORIENTED_EDGE('',*,*,#9717,.T.);
#13896=ORIENTED_EDGE('',*,*,#9722,.T.);
#13897=ORIENTED_EDGE('',*,*,#9723,.F.);
#13898=ORIENTED_EDGE('',*,*,#9724,.F.);
#13899=ORIENTED_EDGE('',*,*,#9725,.F.);
#13900=ORIENTED_EDGE('',*,*,#9726,.F.);
#13901=ORIENTED_EDGE('',*,*,#9727,.T.);
#13902=ORIENTED_EDGE('',*,*,#9724,.T.);
#13903=ORIENTED_EDGE('',*,*,#9728,.T.);
#13904=ORIENTED_EDGE('',*,*,#9729,.F.);
#13905=ORIENTED_EDGE('',*,*,#9730,.F.);
#13906=ORIENTED_EDGE('',*,*,#9731,.F.);
#13907=ORIENTED_EDGE('',*,*,#9732,.F.);
#13908=ORIENTED_EDGE('',*,*,#9733,.T.);
#13909=ORIENTED_EDGE('',*,*,#9730,.T.);
#13910=ORIENTED_EDGE('',*,*,#9734,.T.);
#13911=ORIENTED_EDGE('',*,*,#9715,.T.);
#13912=ORIENTED_EDGE('',*,*,#9735,.T.);
#13913=ORIENTED_EDGE('',*,*,#9731,.T.);
#13914=ORIENTED_EDGE('',*,*,#9736,.T.);
#13915=ORIENTED_EDGE('',*,*,#9729,.T.);
#13916=ORIENTED_EDGE('',*,*,#9737,.T.);
#13917=ORIENTED_EDGE('',*,*,#9725,.T.);
#13918=ORIENTED_EDGE('',*,*,#9738,.T.);
#13919=ORIENTED_EDGE('',*,*,#9723,.T.);
#13920=ORIENTED_EDGE('',*,*,#9739,.T.);
#13921=ORIENTED_EDGE('',*,*,#9711,.T.);
#13922=ORIENTED_EDGE('',*,*,#9740,.T.);
#13923=ORIENTED_EDGE('',*,*,#9709,.T.);
#13924=ORIENTED_EDGE('',*,*,#9741,.T.);
#13925=ORIENTED_EDGE('',*,*,#9697,.T.);
#13926=ORIENTED_EDGE('',*,*,#9742,.T.);
#13927=ORIENTED_EDGE('',*,*,#9700,.F.);
#13928=ORIENTED_EDGE('',*,*,#9708,.F.);
#13929=ORIENTED_EDGE('',*,*,#9705,.F.);
#13930=ORIENTED_EDGE('',*,*,#9743,.F.);
#13931=ORIENTED_EDGE('',*,*,#9706,.F.);
#13932=ORIENTED_EDGE('',*,*,#9722,.F.);
#13933=ORIENTED_EDGE('',*,*,#9719,.F.);
#13934=ORIENTED_EDGE('',*,*,#9744,.F.);
#13935=ORIENTED_EDGE('',*,*,#9720,.F.);
#13936=ORIENTED_EDGE('',*,*,#9736,.F.);
#13937=ORIENTED_EDGE('',*,*,#9733,.F.);
#13938=ORIENTED_EDGE('',*,*,#9745,.F.);
#13939=ORIENTED_EDGE('',*,*,#9707,.F.);
#13940=ORIENTED_EDGE('',*,*,#9741,.F.);
#13941=ORIENTED_EDGE('',*,*,#9739,.F.);
#13942=ORIENTED_EDGE('',*,*,#9737,.F.);
#13943=ORIENTED_EDGE('',*,*,#9735,.F.);
#13944=ORIENTED_EDGE('',*,*,#9721,.F.);
#13945=ORIENTED_EDGE('',*,*,#9746,.F.);
#13946=ORIENTED_EDGE('',*,*,#9747,.F.);
#13947=ORIENTED_EDGE('',*,*,#9748,.F.);
#13948=ORIENTED_EDGE('',*,*,#9749,.F.);
#13949=ORIENTED_EDGE('',*,*,#9750,.F.);
#13950=ORIENTED_EDGE('',*,*,#9751,.F.);
#13951=ORIENTED_EDGE('',*,*,#9749,.T.);
#13952=ORIENTED_EDGE('',*,*,#9752,.T.);
#13953=ORIENTED_EDGE('',*,*,#9753,.T.);
#13954=ORIENTED_EDGE('',*,*,#9754,.F.);
#13955=ORIENTED_EDGE('',*,*,#9748,.T.);
#13956=ORIENTED_EDGE('',*,*,#9755,.T.);
#13957=ORIENTED_EDGE('',*,*,#9756,.T.);
#13958=ORIENTED_EDGE('',*,*,#9752,.F.);
#13959=ORIENTED_EDGE('',*,*,#9746,.T.);
#13960=ORIENTED_EDGE('',*,*,#9757,.T.);
#13961=ORIENTED_EDGE('',*,*,#9758,.T.);
#13962=ORIENTED_EDGE('',*,*,#9759,.T.);
#13963=ORIENTED_EDGE('',*,*,#9760,.T.);
#13964=ORIENTED_EDGE('',*,*,#9757,.F.);
#13965=ORIENTED_EDGE('',*,*,#9751,.T.);
#13966=ORIENTED_EDGE('',*,*,#9761,.T.);
#13967=ORIENTED_EDGE('',*,*,#9747,.T.);
#13968=ORIENTED_EDGE('',*,*,#9759,.F.);
#13969=ORIENTED_EDGE('',*,*,#9762,.T.);
#13970=ORIENTED_EDGE('',*,*,#9755,.F.);
#13971=ORIENTED_EDGE('',*,*,#9763,.T.);
#13972=ORIENTED_EDGE('',*,*,#9761,.F.);
#13973=ORIENTED_EDGE('',*,*,#9750,.T.);
#13974=ORIENTED_EDGE('',*,*,#9754,.T.);
#13975=ORIENTED_EDGE('',*,*,#9756,.F.);
#13976=ORIENTED_EDGE('',*,*,#9764,.T.);
#13977=ORIENTED_EDGE('',*,*,#9765,.T.);
#13978=ORIENTED_EDGE('',*,*,#9766,.F.);
#13979=ORIENTED_EDGE('',*,*,#9762,.F.);
#13980=ORIENTED_EDGE('',*,*,#9767,.T.);
#13981=ORIENTED_EDGE('',*,*,#9768,.T.);
#13982=ORIENTED_EDGE('',*,*,#9764,.F.);
#13983=ORIENTED_EDGE('',*,*,#9758,.F.);
#13984=ORIENTED_EDGE('',*,*,#9769,.T.);
#13985=ORIENTED_EDGE('',*,*,#9770,.T.);
#13986=ORIENTED_EDGE('',*,*,#9767,.F.);
#13987=ORIENTED_EDGE('',*,*,#9771,.F.);
#13988=ORIENTED_EDGE('',*,*,#9772,.F.);
#13989=ORIENTED_EDGE('',*,*,#9672,.F.);
#13990=ORIENTED_EDGE('',*,*,#9669,.F.);
#13991=ORIENTED_EDGE('',*,*,#9666,.F.);
#13992=ORIENTED_EDGE('',*,*,#9663,.F.);
#13993=ORIENTED_EDGE('',*,*,#9660,.F.);
#13994=ORIENTED_EDGE('',*,*,#9657,.F.);
#13995=ORIENTED_EDGE('',*,*,#9654,.F.);
#13996=ORIENTED_EDGE('',*,*,#9773,.F.);
#13997=ORIENTED_EDGE('',*,*,#9774,.T.);
#13998=ORIENTED_EDGE('',*,*,#9694,.T.);
#13999=ORIENTED_EDGE('',*,*,#9691,.T.);
#14000=ORIENTED_EDGE('',*,*,#9688,.T.);
#14001=ORIENTED_EDGE('',*,*,#9685,.T.);
#14002=ORIENTED_EDGE('',*,*,#9682,.T.);
#14003=ORIENTED_EDGE('',*,*,#9679,.T.);
#14004=ORIENTED_EDGE('',*,*,#9775,.T.);
#14005=ORIENTED_EDGE('',*,*,#9776,.T.);
#14006=ORIENTED_EDGE('',*,*,#9777,.T.);
#14007=ORIENTED_EDGE('',*,*,#9778,.T.);
#14008=ORIENTED_EDGE('',*,*,#9773,.T.);
#14009=ORIENTED_EDGE('',*,*,#9692,.T.);
#14010=ORIENTED_EDGE('',*,*,#9774,.F.);
#14011=ORIENTED_EDGE('',*,*,#9778,.F.);
#14012=ORIENTED_EDGE('',*,*,#9779,.T.);
#14013=ORIENTED_EDGE('',*,*,#9780,.F.);
#14014=ORIENTED_EDGE('',*,*,#9674,.F.);
#14015=ORIENTED_EDGE('',*,*,#9677,.F.);
#14016=ORIENTED_EDGE('',*,*,#9681,.F.);
#14017=ORIENTED_EDGE('',*,*,#9684,.F.);
#14018=ORIENTED_EDGE('',*,*,#9687,.F.);
#14019=ORIENTED_EDGE('',*,*,#9690,.F.);
#14020=ORIENTED_EDGE('',*,*,#9693,.F.);
#14021=ORIENTED_EDGE('',*,*,#9779,.F.);
#14022=ORIENTED_EDGE('',*,*,#9777,.F.);
#14023=ORIENTED_EDGE('',*,*,#9652,.F.);
#14024=ORIENTED_EDGE('',*,*,#9656,.F.);
#14025=ORIENTED_EDGE('',*,*,#9659,.F.);
#14026=ORIENTED_EDGE('',*,*,#9662,.F.);
#14027=ORIENTED_EDGE('',*,*,#9665,.F.);
#14028=ORIENTED_EDGE('',*,*,#9668,.F.);
#14029=ORIENTED_EDGE('',*,*,#9671,.F.);
#14030=ORIENTED_EDGE('',*,*,#9781,.F.);
#14031=ORIENTED_EDGE('',*,*,#9771,.T.);
#14032=ORIENTED_EDGE('',*,*,#9678,.T.);
#14033=ORIENTED_EDGE('',*,*,#9675,.T.);
#14034=ORIENTED_EDGE('',*,*,#9780,.T.);
#14035=ORIENTED_EDGE('',*,*,#9782,.T.);
#14036=ORIENTED_EDGE('',*,*,#9783,.F.);
#14037=ORIENTED_EDGE('',*,*,#9760,.F.);
#14038=ORIENTED_EDGE('',*,*,#9784,.T.);
#14039=ORIENTED_EDGE('',*,*,#9785,.T.);
#14040=ORIENTED_EDGE('',*,*,#9769,.F.);
#14041=ORIENTED_EDGE('',*,*,#9763,.F.);
#14042=ORIENTED_EDGE('',*,*,#9786,.T.);
#14043=ORIENTED_EDGE('',*,*,#9787,.T.);
#14044=ORIENTED_EDGE('',*,*,#9784,.F.);
#14045=ORIENTED_EDGE('',*,*,#9753,.F.);
#14046=ORIENTED_EDGE('',*,*,#9766,.T.);
#14047=ORIENTED_EDGE('',*,*,#9788,.T.);
#14048=ORIENTED_EDGE('',*,*,#9786,.F.);
#14049=ORIENTED_EDGE('',*,*,#9768,.F.);
#14050=ORIENTED_EDGE('',*,*,#9770,.F.);
#14051=ORIENTED_EDGE('',*,*,#9785,.F.);
#14052=ORIENTED_EDGE('',*,*,#9787,.F.);
#14053=ORIENTED_EDGE('',*,*,#9788,.F.);
#14054=ORIENTED_EDGE('',*,*,#9765,.F.);
#14055=ORIENTED_EDGE('',*,*,#9727,.F.);
#14056=ORIENTED_EDGE('',*,*,#9789,.F.);
#14057=ORIENTED_EDGE('',*,*,#9734,.F.);
#14058=ORIENTED_EDGE('',*,*,#9738,.F.);
#14059=ORIENTED_EDGE('',*,*,#9713,.F.);
#14060=ORIENTED_EDGE('',*,*,#9790,.F.);
#14061=ORIENTED_EDGE('',*,*,#9728,.F.);
#14062=ORIENTED_EDGE('',*,*,#9740,.F.);
#14063=ORIENTED_EDGE('',*,*,#9699,.F.);
#14064=ORIENTED_EDGE('',*,*,#9791,.F.);
#14065=ORIENTED_EDGE('',*,*,#9714,.F.);
#14066=ORIENTED_EDGE('',*,*,#9742,.F.);
#14067=ORIENTED_EDGE('',*,*,#9792,.T.);
#14068=ORIENTED_EDGE('',*,*,#9698,.T.);
#14069=ORIENTED_EDGE('',*,*,#9743,.T.);
#14070=ORIENTED_EDGE('',*,*,#9704,.T.);
#14071=ORIENTED_EDGE('',*,*,#9744,.T.);
#14072=ORIENTED_EDGE('',*,*,#9718,.T.);
#14073=ORIENTED_EDGE('',*,*,#9745,.T.);
#14074=ORIENTED_EDGE('',*,*,#9732,.T.);
#14075=ORIENTED_EDGE('',*,*,#9789,.T.);
#14076=ORIENTED_EDGE('',*,*,#9726,.T.);
#14077=ORIENTED_EDGE('',*,*,#9790,.T.);
#14078=ORIENTED_EDGE('',*,*,#9712,.T.);
#14079=ORIENTED_EDGE('',*,*,#9791,.T.);
#14080=ORIENTED_EDGE('',*,*,#9793,.F.);
#14081=ORIENTED_EDGE('',*,*,#9794,.T.);
#14082=ORIENTED_EDGE('',*,*,#9792,.F.);
#14083=ORIENTED_EDGE('',*,*,#9795,.T.);
#14084=ORIENTED_EDGE('',*,*,#9793,.T.);
#14085=ORIENTED_EDGE('',*,*,#9795,.F.);
#14086=ORIENTED_EDGE('',*,*,#9796,.F.);
#14087=ORIENTED_EDGE('',*,*,#9775,.F.);
#14088=ORIENTED_EDGE('',*,*,#9653,.F.);
#14089=ORIENTED_EDGE('',*,*,#9776,.F.);
#14090=ORIENTED_EDGE('',*,*,#9797,.T.);
#14091=ORIENTED_EDGE('',*,*,#9796,.T.);
#14092=ORIENTED_EDGE('',*,*,#9797,.F.);
#14093=ORIENTED_EDGE('',*,*,#9670,.T.);
#14094=ORIENTED_EDGE('',*,*,#9772,.T.);
#14095=ORIENTED_EDGE('',*,*,#9782,.F.);
#14096=ORIENTED_EDGE('',*,*,#9781,.T.);
#14097=ORIENTED_EDGE('',*,*,#9794,.F.);
#14098=ORIENTED_EDGE('',*,*,#9798,.T.);
#14099=ORIENTED_EDGE('',*,*,#9783,.T.);
#14100=ORIENTED_EDGE('',*,*,#9798,.F.);
#14101=CONICAL_SURFACE('',#15254,14.75,0.785398163397448);
#14102=CONICAL_SURFACE('',#15262,7.4,0.785398163397448);
#14103=CONICAL_SURFACE('',#15271,14.75,0.785398163397448);
#14104=CONICAL_SURFACE('',#15279,7.4,0.785398163397448);
#14105=CONICAL_SURFACE('',#15288,9.3,0.785398163397448);
#14106=CONICAL_SURFACE('',#15292,6.3,0.785398163397439);
#14107=CONICAL_SURFACE('',#15306,6.3,0.785398163397439);
#14108=CONICAL_SURFACE('',#15310,6.3,0.785398163397439);
#14109=CONICAL_SURFACE('',#15314,6.3,0.785398163397439);
#14110=CONICAL_SURFACE('',#15318,62.25,0.785398163397446);
#14111=CONICAL_SURFACE('',#15328,62.25,0.785398163397446);
#14112=CONICAL_SURFACE('',#15337,62.25,0.785398163397455);
#14113=CONICAL_SURFACE('',#15347,62.25,0.785398163397455);
#14114=CONICAL_SURFACE('',#15356,7.4,0.785398163397449);
#14115=CONICAL_SURFACE('',#15365,7.4,0.785398163397449);
#14116=CONICAL_SURFACE('',#15495,13.25,0.785398163397442);
#14117=CONICAL_SURFACE('',#15503,19.25,0.785398163397457);
#14118=CONICAL_SURFACE('',#15513,6.3,0.785398163397435);
#14119=CONICAL_SURFACE('',#15516,6.3,0.785398163397435);
#14120=CONICAL_SURFACE('',#15525,6.3,0.785398163397442);
#14121=CONICAL_SURFACE('',#15527,6.3,0.785398163397442);
#14122=CONICAL_SURFACE('',#15536,6.3,0.785398163397435);
#14123=CONICAL_SURFACE('',#15539,6.3,0.785398163397438);
#14124=CONICAL_SURFACE('',#15544,6.3,0.785398163397442);
#14125=CONICAL_SURFACE('',#15546,6.3,0.785398163397442);
#14126=CONICAL_SURFACE('',#15555,1.75,0.785398163397441);
#14127=CONICAL_SURFACE('',#15560,1.75,0.785398163397441);
#14128=CONICAL_SURFACE('',#15577,5.30000000000001,0.785398163397457);
#14129=CONICAL_SURFACE('',#15587,5.29999999999999,0.785398163397457);
#14130=CONICAL_SURFACE('',#15591,5.29999999999999,0.785398163397457);
#14131=CONICAL_SURFACE('',#15595,5.30000000000001,0.785398163397457);
#14132=CONICAL_SURFACE('',#15599,9.75,0.785398163397457);
#14133=CONICAL_SURFACE('',#15826,41.4267766952966,1.17809724509617);
#14134=CONICAL_SURFACE('',#15839,42.,0.785398163397448);
#14135=CONICAL_SURFACE('',#15953,10.85,0.785398163397446);
#14136=CONICAL_SURFACE('',#15961,10.85,0.785398163397448);
#14137=CONICAL_SURFACE('',#15969,10.85,0.785398163397448);
#14138=CONICAL_SURFACE('',#15977,10.85,0.785398163397448);
#14139=CONICAL_SURFACE('',#15986,10.85,0.785398163397448);
#14140=CONICAL_SURFACE('',#15990,10.85,0.463647609000803);
#14141=CONICAL_SURFACE('',#16018,10.85,0.785398163397448);
#14142=CONICAL_SURFACE('',#16025,10.85,0.785398163397448);
#14143=CONICAL_SURFACE('',#16056,10.85,0.785398163397446);
#14144=CONICAL_SURFACE('',#16063,10.85,0.785398163397448);
#14145=CONICAL_SURFACE('',#16070,10.85,0.785398163397448);
#14146=CONICAL_SURFACE('',#16077,10.85,0.785398163397448);
#14147=CONICAL_SURFACE('',#16084,10.85,0.785398163397448);
#14148=CONICAL_SURFACE('',#16088,10.85,0.463647609000803);
#14149=CONICAL_SURFACE('',#16094,10.85,0.785398163397446);
#14150=CONICAL_SURFACE('',#16098,10.85,0.463647609000803);
#14151=CONICAL_SURFACE('',#16100,3.6,0.78539816339745);
#14152=CONICAL_SURFACE('',#16125,10.85,0.463647609000803);
#14153=CONICAL_SURFACE('',#16126,10.85,0.463647609000803);
#14154=CONICAL_SURFACE('',#16127,10.85,0.463647609000803);
#14155=CONICAL_SURFACE('',#16128,10.85,0.463647609000803);
#14156=CONICAL_SURFACE('',#16130,10.85,0.463647609000803);
#14157=CONICAL_SURFACE('',#16131,10.85,0.463647609000803);
#14158=CONICAL_SURFACE('',#16132,10.85,0.463647609000803);
#14159=CONICAL_SURFACE('',#16133,10.85,0.463647609000803);
#14160=CONICAL_SURFACE('',#16134,10.85,0.463647609000803);
#14161=CONICAL_SURFACE('',#16136,10.85,0.463647609000803);
#14162=CONICAL_SURFACE('',#16149,12.25,0.785398163397442);
#14163=CONICAL_SURFACE('',#16172,19.15,0.404891786285086);
#14164=CONICAL_SURFACE('',#16177,23.9,0.278299659005112);
#14165=CONICAL_SURFACE('',#16181,27.3,0.785398163397449);
#14166=CONICAL_SURFACE('',#16185,27.3,0.785398163397448);
#14167=CONICAL_SURFACE('',#16189,23.9,0.278299659005111);
#14168=CONICAL_SURFACE('',#16193,19.15,0.404891786285086);
#14169=CONICAL_SURFACE('',#16197,15.2,0.785398163397448);
#14170=CONICAL_SURFACE('',#16201,15.2,0.785398163397449);
#14171=CONICAL_SURFACE('',#16230,20.64,0.785398163397448);
#14172=CONICAL_SURFACE('',#16238,16.9764870412073,1.27679502502111);
#14173=CONICAL_SURFACE('',#16244,17.75,0.982793723247329);
#14174=CONICAL_SURFACE('',#16253,16.5,0.982793723247329);
#14175=CONICAL_SURFACE('',#16255,4.25,0.78539816339745);
#14176=CONICAL_SURFACE('',#16273,8.25,0.78539816339745);
#14177=CONICAL_SURFACE('',#16277,8.25,0.78539816339745);
#14178=CONICAL_SURFACE('',#16285,10.75,0.785398163397449);
#14179=CONICAL_SURFACE('',#16305,40.9,0.785398163397437);
#14180=CONICAL_SURFACE('',#16356,40.75,0.785398163397447);
#14181=CONICAL_SURFACE('',#16660,5.75,0.78539816339745);
#14182=CONICAL_SURFACE('',#16667,8.75,0.785398163397448);
#14183=CONICAL_SURFACE('',#16742,8.75,0.785398163397448);
#14184=ADVANCED_FACE('',(#1617),#14101,.T.);
#14185=ADVANCED_FACE('',(#1618),#1366,.T.);
#14186=ADVANCED_FACE('',(#1619,#417),#558,.F.);
#14187=ADVANCED_FACE('',(#1620),#14102,.F.);
#14188=ADVANCED_FACE('',(#1621,#418),#559,.T.);
#14189=ADVANCED_FACE('',(#1622),#1367,.F.);
#14190=ADVANCED_FACE('',(#1623),#14103,.T.);
#14191=ADVANCED_FACE('',(#1624,#419),#560,.T.);
#14192=ADVANCED_FACE('',(#1625),#1368,.T.);
#14193=ADVANCED_FACE('',(#1626),#14104,.F.);
#14194=ADVANCED_FACE('',(#1627,#420),#561,.T.);
#14195=ADVANCED_FACE('',(#1628),#1369,.F.);
#14196=ADVANCED_FACE('',(#1629),#14105,.F.);
#14197=ADVANCED_FACE('',(#1630),#1370,.F.);
#14198=ADVANCED_FACE('',(#1631),#14106,.F.);
#14199=ADVANCED_FACE('',(#1632,#421,#422,#423,#424,#425),#562,.T.);
#14200=ADVANCED_FACE('',(#1633),#1371,.F.);
#14201=ADVANCED_FACE('',(#1634),#14107,.F.);
#14202=ADVANCED_FACE('',(#1635),#1372,.F.);
#14203=ADVANCED_FACE('',(#1636),#14108,.F.);
#14204=ADVANCED_FACE('',(#1637),#1373,.F.);
#14205=ADVANCED_FACE('',(#1638),#14109,.F.);
#14206=ADVANCED_FACE('',(#1639),#1374,.F.);
#14207=ADVANCED_FACE('',(#1640),#14110,.T.);
#14208=ADVANCED_FACE('',(#1641),#563,.T.);
#14209=ADVANCED_FACE('',(#1642),#564,.T.);
#14210=ADVANCED_FACE('',(#1643),#565,.T.);
#14211=ADVANCED_FACE('',(#1644),#566,.T.);
#14212=ADVANCED_FACE('',(#1645),#567,.T.);
#14213=ADVANCED_FACE('',(#1646),#14111,.T.);
#14214=ADVANCED_FACE('',(#1647),#568,.T.);
#14215=ADVANCED_FACE('',(#1648),#1375,.T.);
#14216=ADVANCED_FACE('',(#1649),#14112,.T.);
#14217=ADVANCED_FACE('',(#1650),#569,.T.);
#14218=ADVANCED_FACE('',(#1651),#570,.T.);
#14219=ADVANCED_FACE('',(#1652),#571,.T.);
#14220=ADVANCED_FACE('',(#1653),#572,.T.);
#14221=ADVANCED_FACE('',(#1654),#573,.T.);
#14222=ADVANCED_FACE('',(#1655),#14113,.T.);
#14223=ADVANCED_FACE('',(#1656),#574,.T.);
#14224=ADVANCED_FACE('',(#1657),#1376,.T.);
#14225=ADVANCED_FACE('',(#1658),#14114,.F.);
#14226=ADVANCED_FACE('',(#1659,#426,#427,#428),#575,.F.);
#14227=ADVANCED_FACE('',(#1660),#14115,.F.);
#14228=ADVANCED_FACE('',(#1661),#256,.T.);
#14229=ADVANCED_FACE('',(#1662),#1377,.T.);
#14230=ADVANCED_FACE('',(#1663),#257,.T.);
#14231=ADVANCED_FACE('',(#1664),#1378,.T.);
#14232=ADVANCED_FACE('',(#1665),#258,.T.);
#14233=ADVANCED_FACE('',(#1666),#259,.T.);
#14234=ADVANCED_FACE('',(#1667),#1379,.T.);
#14235=ADVANCED_FACE('',(#1668),#1380,.T.);
#14236=ADVANCED_FACE('',(#1669),#1381,.T.);
#14237=ADVANCED_FACE('',(#1670),#576,.T.);
#14238=ADVANCED_FACE('',(#1671),#260,.T.);
#14239=ADVANCED_FACE('',(#1672),#1382,.T.);
#14240=ADVANCED_FACE('',(#1673),#261,.T.);
#14241=ADVANCED_FACE('',(#1674),#1383,.T.);
#14242=ADVANCED_FACE('',(#1675),#577,.T.);
#14243=ADVANCED_FACE('',(#1676),#1384,.T.);
#14244=ADVANCED_FACE('',(#1677),#578,.T.);
#14245=ADVANCED_FACE('',(#1678),#262,.T.);
#14246=ADVANCED_FACE('',(#1679),#1385,.T.);
#14247=ADVANCED_FACE('',(#1680),#263,.T.);
#14248=ADVANCED_FACE('',(#1681),#1386,.T.);
#14249=ADVANCED_FACE('',(#1682),#579,.T.);
#14250=ADVANCED_FACE('',(#1683),#264,.T.);
#14251=ADVANCED_FACE('',(#1684),#1387,.T.);
#14252=ADVANCED_FACE('',(#1685),#1388,.T.);
#14253=ADVANCED_FACE('',(#1686),#265,.T.);
#14254=ADVANCED_FACE('',(#1687),#1389,.T.);
#14255=ADVANCED_FACE('',(#1688),#580,.F.);
#14256=ADVANCED_FACE('',(#1689),#266,.T.);
#14257=ADVANCED_FACE('',(#1690),#1390,.T.);
#14258=ADVANCED_FACE('',(#1691),#1391,.T.);
#14259=ADVANCED_FACE('',(#1692),#581,.F.);
#14260=ADVANCED_FACE('',(#1693),#1392,.T.);
#14261=ADVANCED_FACE('',(#1694),#267,.T.);
#14262=ADVANCED_FACE('',(#1695),#1393,.T.);
#14263=ADVANCED_FACE('',(#1696),#582,.F.);
#14264=ADVANCED_FACE('',(#1697),#1394,.T.);
#14265=ADVANCED_FACE('',(#1698),#268,.T.);
#14266=ADVANCED_FACE('',(#1699),#1395,.T.);
#14267=ADVANCED_FACE('',(#1700),#583,.F.);
#14268=ADVANCED_FACE('',(#1701),#1396,.T.);
#14269=ADVANCED_FACE('',(#1702),#269,.T.);
#14270=ADVANCED_FACE('',(#1703),#1397,.T.);
#14271=ADVANCED_FACE('',(#1704),#270,.T.);
#14272=ADVANCED_FACE('',(#1705),#1398,.T.);
#14273=ADVANCED_FACE('',(#1706),#271,.T.);
#14274=ADVANCED_FACE('',(#1707),#1399,.T.);
#14275=ADVANCED_FACE('',(#1708),#272,.T.);
#14276=ADVANCED_FACE('',(#1709),#1400,.T.);
#14277=ADVANCED_FACE('',(#1710),#1401,.T.);
#14278=ADVANCED_FACE('',(#1711),#273,.T.);
#14279=ADVANCED_FACE('',(#1712,#429,#430),#1402,.F.);
#14280=ADVANCED_FACE('',(#1713),#207,.F.);
#14281=ADVANCED_FACE('',(#1714),#208,.F.);
#14282=ADVANCED_FACE('',(#1715),#209,.F.);
#14283=ADVANCED_FACE('',(#1716),#210,.F.);
#14284=ADVANCED_FACE('',(#1717),#211,.F.);
#14285=ADVANCED_FACE('',(#1718),#212,.F.);
#14286=ADVANCED_FACE('',(#1719),#213,.F.);
#14287=ADVANCED_FACE('',(#1720),#214,.F.);
#14288=ADVANCED_FACE('',(#1721),#1403,.F.);
#14289=ADVANCED_FACE('',(#1722),#584,.T.);
#14290=ADVANCED_FACE('',(#1723),#585,.T.);
#14291=ADVANCED_FACE('',(#1724),#586,.T.);
#14292=ADVANCED_FACE('',(#1725),#587,.T.);
#14293=ADVANCED_FACE('',(#1726),#1404,.F.);
#14294=ADVANCED_FACE('',(#1727,#431),#588,.F.);
#14295=ADVANCED_FACE('',(#1728),#1405,.F.);
#14296=ADVANCED_FACE('',(#1729,#432),#589,.F.);
#14297=ADVANCED_FACE('',(#1730),#1406,.F.);
#14298=ADVANCED_FACE('',(#1731,#433),#590,.F.);
#14299=ADVANCED_FACE('',(#1732,#434),#591,.T.);
#14300=ADVANCED_FACE('',(#1733),#1407,.T.);
#14301=ADVANCED_FACE('',(#1734),#1408,.T.);
#14302=ADVANCED_FACE('',(#1735),#592,.T.);
#14303=ADVANCED_FACE('',(#1736),#593,.T.);
#14304=ADVANCED_FACE('',(#1737),#14116,.F.);
#14305=ADVANCED_FACE('',(#1738,#435),#594,.F.);
#14306=ADVANCED_FACE('',(#1739),#1409,.F.);
#14307=ADVANCED_FACE('',(#1740),#14117,.F.);
#14308=ADVANCED_FACE('',(#1741,#436),#595,.T.);
#14309=ADVANCED_FACE('',(#1742),#1410,.F.);
#14310=ADVANCED_FACE('',(#1743),#14118,.F.);
#14311=ADVANCED_FACE('',(#1744),#215,.T.);
#14312=ADVANCED_FACE('',(#1745),#216,.T.);
#14313=ADVANCED_FACE('',(#1746),#14119,.F.);
#14314=ADVANCED_FACE('',(#1747),#217,.T.);
#14315=ADVANCED_FACE('',(#1748),#218,.T.);
#14316=ADVANCED_FACE('',(#1749),#219,.T.);
#14317=ADVANCED_FACE('',(#1750),#220,.T.);
#14318=ADVANCED_FACE('',(#1751),#596,.T.);
#14319=ADVANCED_FACE('',(#1752),#1411,.T.);
#14320=ADVANCED_FACE('',(#1753),#1412,.F.);
#14321=ADVANCED_FACE('',(#1754),#14120,.F.);
#14322=ADVANCED_FACE('',(#1755),#221,.T.);
#14323=ADVANCED_FACE('',(#1756),#222,.T.);
#14324=ADVANCED_FACE('',(#1757),#14121,.F.);
#14325=ADVANCED_FACE('',(#1758),#223,.T.);
#14326=ADVANCED_FACE('',(#1759),#224,.T.);
#14327=ADVANCED_FACE('',(#1760),#225,.T.);
#14328=ADVANCED_FACE('',(#1761),#226,.T.);
#14329=ADVANCED_FACE('',(#1762),#597,.T.);
#14330=ADVANCED_FACE('',(#1763),#1413,.T.);
#14331=ADVANCED_FACE('',(#1764),#1414,.F.);
#14332=ADVANCED_FACE('',(#1765),#14122,.F.);
#14333=ADVANCED_FACE('',(#1766),#227,.T.);
#14334=ADVANCED_FACE('',(#1767),#228,.T.);
#14335=ADVANCED_FACE('',(#1768),#14123,.F.);
#14336=ADVANCED_FACE('',(#1769),#229,.T.);
#14337=ADVANCED_FACE('',(#1770),#230,.T.);
#14338=ADVANCED_FACE('',(#1771),#231,.T.);
#14339=ADVANCED_FACE('',(#1772),#232,.T.);
#14340=ADVANCED_FACE('',(#1773),#1415,.F.);
#14341=ADVANCED_FACE('',(#1774),#14124,.F.);
#14342=ADVANCED_FACE('',(#1775),#233,.T.);
#14343=ADVANCED_FACE('',(#1776),#234,.T.);
#14344=ADVANCED_FACE('',(#1777),#14125,.F.);
#14345=ADVANCED_FACE('',(#1778),#235,.T.);
#14346=ADVANCED_FACE('',(#1779),#236,.T.);
#14347=ADVANCED_FACE('',(#1780),#237,.T.);
#14348=ADVANCED_FACE('',(#1781),#238,.T.);
#14349=ADVANCED_FACE('',(#1782),#598,.T.);
#14350=ADVANCED_FACE('',(#1783),#1416,.T.);
#14351=ADVANCED_FACE('',(#1784),#1417,.F.);
#14352=ADVANCED_FACE('',(#1785),#239,.T.);
#14353=ADVANCED_FACE('',(#1786),#240,.T.);
#14354=ADVANCED_FACE('',(#1787),#241,.T.);
#14355=ADVANCED_FACE('',(#1788),#14126,.T.);
#14356=ADVANCED_FACE('',(#1789),#242,.T.);
#14357=ADVANCED_FACE('',(#1790),#243,.F.);
#14358=ADVANCED_FACE('',(#1791),#1418,.T.);
#14359=ADVANCED_FACE('',(#1792),#244,.T.);
#14360=ADVANCED_FACE('',(#1793),#245,.T.);
#14361=ADVANCED_FACE('',(#1794),#246,.T.);
#14362=ADVANCED_FACE('',(#1795),#14127,.T.);
#14363=ADVANCED_FACE('',(#1796),#247,.T.);
#14364=ADVANCED_FACE('',(#1797),#248,.F.);
#14365=ADVANCED_FACE('',(#1798),#274,.T.);
#14366=ADVANCED_FACE('',(#1799),#599,.T.);
#14367=ADVANCED_FACE('',(#1800),#14128,.F.);
#14368=ADVANCED_FACE('',(#1801,#437,#438,#439,#440,#441),#600,.T.);
#14369=ADVANCED_FACE('',(#1802),#1419,.F.);
#14370=ADVANCED_FACE('',(#1803),#14129,.F.);
#14371=ADVANCED_FACE('',(#1804),#1420,.F.);
#14372=ADVANCED_FACE('',(#1805),#14130,.F.);
#14373=ADVANCED_FACE('',(#1806),#1421,.F.);
#14374=ADVANCED_FACE('',(#1807),#14131,.F.);
#14375=ADVANCED_FACE('',(#1808),#1422,.F.);
#14376=ADVANCED_FACE('',(#1809),#14132,.F.);
#14377=ADVANCED_FACE('',(#1810),#1423,.F.);
#14378=ADVANCED_FACE('',(#1811),#249,.F.);
#14379=ADVANCED_FACE('',(#1812),#1424,.F.);
#14380=ADVANCED_FACE('',(#1813),#1425,.T.);
#14381=ADVANCED_FACE('',(#1814),#132,.T.);
#14382=ADVANCED_FACE('',(#1815),#1426,.T.);
#14383=ADVANCED_FACE('',(#1816),#1427,.T.);
#14384=ADVANCED_FACE('',(#1817),#1428,.T.);
#14385=ADVANCED_FACE('',(#1818),#133,.T.);
#14386=ADVANCED_FACE('',(#1819),#1429,.T.);
#14387=ADVANCED_FACE('',(#1820),#134,.T.);
#14388=ADVANCED_FACE('',(#1821),#601,.F.);
#14389=ADVANCED_FACE('',(#1822),#1430,.T.);
#14390=ADVANCED_FACE('',(#1823),#1431,.T.);
#14391=ADVANCED_FACE('',(#1824),#135,.T.);
#14392=ADVANCED_FACE('',(#1825),#136,.T.);
#14393=ADVANCED_FACE('',(#1826),#1432,.T.);
#14394=ADVANCED_FACE('',(#1827),#1433,.T.);
#14395=ADVANCED_FACE('',(#1828),#137,.T.);
#14396=ADVANCED_FACE('',(#1829),#138,.T.);
#14397=ADVANCED_FACE('',(#1830),#1434,.T.);
#14398=ADVANCED_FACE('',(#1831),#1435,.T.);
#14399=ADVANCED_FACE('',(#1832),#602,.F.);
#14400=ADVANCED_FACE('',(#1833),#603,.T.);
#14401=ADVANCED_FACE('',(#1834,#442,#443,#444,#445,#446),#604,.F.);
#14402=ADVANCED_FACE('',(#1835),#275,.T.);
#14403=ADVANCED_FACE('',(#1836),#1436,.F.);
#14404=ADVANCED_FACE('',(#1837),#276,.T.);
#14405=ADVANCED_FACE('',(#1838),#1437,.T.);
#14406=ADVANCED_FACE('',(#1839),#277,.T.);
#14407=ADVANCED_FACE('',(#1840),#250,.F.);
#14408=ADVANCED_FACE('',(#1841),#251,.F.);
#14409=ADVANCED_FACE('',(#1842,#447,#448,#449),#605,.F.);
#14410=ADVANCED_FACE('',(#1843),#278,.T.);
#14411=ADVANCED_FACE('',(#1844,#450),#606,.T.);
#14412=ADVANCED_FACE('',(#1845),#279,.T.);
#14413=ADVANCED_FACE('',(#1846),#1438,.T.);
#14414=ADVANCED_FACE('',(#1847),#280,.T.);
#14415=ADVANCED_FACE('',(#1848,#451),#607,.T.);
#14416=ADVANCED_FACE('',(#1849),#281,.T.);
#14417=ADVANCED_FACE('',(#1850,#452),#608,.T.);
#14418=ADVANCED_FACE('',(#1851),#1439,.T.);
#14419=ADVANCED_FACE('',(#1852),#282,.T.);
#14420=ADVANCED_FACE('',(#1853),#283,.T.);
#14421=ADVANCED_FACE('',(#1854),#1440,.T.);
#14422=ADVANCED_FACE('',(#1855),#609,.T.);
#14423=ADVANCED_FACE('',(#1856),#284,.T.);
#14424=ADVANCED_FACE('',(#1857),#1441,.T.);
#14425=ADVANCED_FACE('',(#1858),#285,.T.);
#14426=ADVANCED_FACE('',(#1859),#139,.T.);
#14427=ADVANCED_FACE('',(#1860),#140,.T.);
#14428=ADVANCED_FACE('',(#1861),#286,.T.);
#14429=ADVANCED_FACE('',(#1862),#1442,.T.);
#14430=ADVANCED_FACE('',(#1863),#1443,.T.);
#14431=ADVANCED_FACE('',(#1864),#610,.T.);
#14432=ADVANCED_FACE('',(#1865),#1444,.T.);
#14433=ADVANCED_FACE('',(#1866),#1445,.T.);
#14434=ADVANCED_FACE('',(#1867),#611,.T.);
#14435=ADVANCED_FACE('',(#1868),#1446,.T.);
#14436=ADVANCED_FACE('',(#1869),#141,.T.);
#14437=ADVANCED_FACE('',(#1870),#287,.T.);
#14438=ADVANCED_FACE('',(#1871),#1447,.T.);
#14439=ADVANCED_FACE('',(#1872),#1448,.T.);
#14440=ADVANCED_FACE('',(#1873),#1449,.F.);
#14441=ADVANCED_FACE('',(#1874),#142,.T.);
#14442=ADVANCED_FACE('',(#1875),#143,.T.);
#14443=ADVANCED_FACE('',(#1876),#144,.T.);
#14444=ADVANCED_FACE('',(#1877),#288,.T.);
#14445=ADVANCED_FACE('',(#1878),#1450,.T.);
#14446=ADVANCED_FACE('',(#1879),#289,.T.);
#14447=ADVANCED_FACE('',(#1880),#1451,.T.);
#14448=ADVANCED_FACE('',(#1881),#290,.T.);
#14449=ADVANCED_FACE('',(#1882),#1452,.T.);
#14450=ADVANCED_FACE('',(#1883),#291,.T.);
#14451=ADVANCED_FACE('',(#1884),#1453,.T.);
#14452=ADVANCED_FACE('',(#1885),#1454,.F.);
#14453=ADVANCED_FACE('',(#1886),#145,.T.);
#14454=ADVANCED_FACE('',(#1887),#292,.T.);
#14455=ADVANCED_FACE('',(#1888),#1455,.T.);
#14456=ADVANCED_FACE('',(#1889),#1456,.F.);
#14457=ADVANCED_FACE('',(#1890),#1457,.F.);
#14458=ADVANCED_FACE('',(#1891),#1458,.F.);
#14459=ADVANCED_FACE('',(#1892),#1459,.F.);
#14460=ADVANCED_FACE('',(#1893),#1460,.F.);
#14461=ADVANCED_FACE('',(#1894,#453),#612,.T.);
#14462=ADVANCED_FACE('',(#1895),#1461,.F.);
#14463=ADVANCED_FACE('',(#1896),#613,.F.);
#14464=ADVANCED_FACE('',(#1897),#614,.F.);
#14465=ADVANCED_FACE('',(#1898),#615,.F.);
#14466=ADVANCED_FACE('',(#1899),#616,.F.);
#14467=ADVANCED_FACE('',(#1900),#617,.F.);
#14468=ADVANCED_FACE('',(#1901),#618,.T.);
#14469=ADVANCED_FACE('',(#1902),#619,.T.);
#14470=ADVANCED_FACE('',(#1903),#620,.T.);
#14471=ADVANCED_FACE('',(#1904),#621,.T.);
#14472=ADVANCED_FACE('',(#1905),#622,.T.);
#14473=ADVANCED_FACE('',(#1906),#1462,.F.);
#14474=ADVANCED_FACE('',(#1907,#454),#623,.F.);
#14475=ADVANCED_FACE('',(#1908),#1463,.F.);
#14476=ADVANCED_FACE('',(#1909),#624,.F.);
#14477=ADVANCED_FACE('',(#1910),#625,.T.);
#14478=ADVANCED_FACE('',(#1911),#626,.T.);
#14479=ADVANCED_FACE('',(#1912),#627,.T.);
#14480=ADVANCED_FACE('',(#1913),#1464,.T.);
#14481=ADVANCED_FACE('',(#1914),#628,.T.);
#14482=ADVANCED_FACE('',(#1915,#455),#629,.T.);
#14483=ADVANCED_FACE('',(#1916),#630,.T.);
#14484=ADVANCED_FACE('',(#1917,#456),#631,.T.);
#14485=ADVANCED_FACE('',(#1918),#632,.T.);
#14486=ADVANCED_FACE('',(#1919),#1465,.T.);
#14487=ADVANCED_FACE('',(#1920),#1466,.F.);
#14488=ADVANCED_FACE('',(#1921),#633,.T.);
#14489=ADVANCED_FACE('',(#1922),#14133,.T.);
#14490=ADVANCED_FACE('',(#1923,#457,#458,#459,#460,#461,#462,#463,#464),
#634,.T.);
#14491=ADVANCED_FACE('',(#1924),#14134,.T.);
#14492=ADVANCED_FACE('',(#1925),#635,.T.);
#14493=ADVANCED_FACE('',(#1926),#636,.T.);
#14494=ADVANCED_FACE('',(#1927),#637,.T.);
#14495=ADVANCED_FACE('',(#1928),#638,.F.);
#14496=ADVANCED_FACE('',(#1929),#639,.F.);
#14497=ADVANCED_FACE('',(#1930),#1467,.F.);
#14498=ADVANCED_FACE('',(#1931),#640,.F.);
#14499=ADVANCED_FACE('',(#1932),#641,.T.);
#14500=ADVANCED_FACE('',(#1933),#642,.T.);
#14501=ADVANCED_FACE('',(#1934),#643,.T.);
#14502=ADVANCED_FACE('',(#1935,#465,#466,#467,#468,#469,#470,#471,#472),
#644,.T.);
#14503=ADVANCED_FACE('',(#1936),#1468,.F.);
#14504=ADVANCED_FACE('',(#1937),#1469,.F.);
#14505=ADVANCED_FACE('',(#1938,#473),#645,.F.);
#14506=ADVANCED_FACE('',(#1939),#1470,.F.);
#14507=ADVANCED_FACE('',(#1940),#1471,.F.);
#14508=ADVANCED_FACE('',(#1941,#474),#646,.F.);
#14509=ADVANCED_FACE('',(#1942),#1472,.F.);
#14510=ADVANCED_FACE('',(#1943),#1473,.F.);
#14511=ADVANCED_FACE('',(#1944,#475),#647,.F.);
#14512=ADVANCED_FACE('',(#1945),#1474,.F.);
#14513=ADVANCED_FACE('',(#1946),#1475,.F.);
#14514=ADVANCED_FACE('',(#1947,#476),#648,.F.);
#14515=ADVANCED_FACE('',(#1948),#1476,.F.);
#14516=ADVANCED_FACE('',(#1949),#1477,.F.);
#14517=ADVANCED_FACE('',(#1950,#477),#649,.F.);
#14518=ADVANCED_FACE('',(#1951),#1478,.F.);
#14519=ADVANCED_FACE('',(#1952),#1479,.F.);
#14520=ADVANCED_FACE('',(#1953,#478),#650,.F.);
#14521=ADVANCED_FACE('',(#1954),#1480,.F.);
#14522=ADVANCED_FACE('',(#1955),#1481,.F.);
#14523=ADVANCED_FACE('',(#1956,#479),#651,.F.);
#14524=ADVANCED_FACE('',(#1957),#1482,.T.);
#14525=ADVANCED_FACE('',(#1958),#652,.T.);
#14526=ADVANCED_FACE('',(#1959),#653,.F.);
#14527=ADVANCED_FACE('',(#1960),#654,.T.);
#14528=ADVANCED_FACE('',(#1961),#655,.T.);
#14529=ADVANCED_FACE('',(#1962),#656,.F.);
#14530=ADVANCED_FACE('',(#1963),#657,.T.);
#14531=ADVANCED_FACE('',(#1964),#658,.T.);
#14532=ADVANCED_FACE('',(#1965),#659,.F.);
#14533=ADVANCED_FACE('',(#1966),#660,.T.);
#14534=ADVANCED_FACE('',(#1967),#661,.T.);
#14535=ADVANCED_FACE('',(#1968),#662,.F.);
#14536=ADVANCED_FACE('',(#1969),#663,.T.);
#14537=ADVANCED_FACE('',(#1970),#1483,.F.);
#14538=ADVANCED_FACE('',(#1971),#1484,.T.);
#14539=ADVANCED_FACE('',(#1972),#1485,.F.);
#14540=ADVANCED_FACE('',(#1973),#1486,.T.);
#14541=ADVANCED_FACE('',(#1974),#1487,.F.);
#14542=ADVANCED_FACE('',(#1975,#480,#481,#482),#664,.T.);
#14543=ADVANCED_FACE('',(#1976),#1488,.T.);
#14544=ADVANCED_FACE('',(#1977,#483,#484,#485),#665,.T.);
#14545=ADVANCED_FACE('',(#1978),#666,.T.);
#14546=ADVANCED_FACE('',(#1979),#667,.T.);
#14547=ADVANCED_FACE('',(#1980),#14135,.T.);
#14548=ADVANCED_FACE('',(#1981),#668,.F.);
#14549=ADVANCED_FACE('',(#1982),#669,.F.);
#14550=ADVANCED_FACE('',(#1983),#670,.F.);
#14551=ADVANCED_FACE('',(#1984),#671,.T.);
#14552=ADVANCED_FACE('',(#1985),#672,.T.);
#14553=ADVANCED_FACE('',(#1986),#14136,.T.);
#14554=ADVANCED_FACE('',(#1987),#673,.F.);
#14555=ADVANCED_FACE('',(#1988),#674,.F.);
#14556=ADVANCED_FACE('',(#1989),#675,.F.);
#14557=ADVANCED_FACE('',(#1990),#676,.T.);
#14558=ADVANCED_FACE('',(#1991),#677,.T.);
#14559=ADVANCED_FACE('',(#1992),#14137,.T.);
#14560=ADVANCED_FACE('',(#1993),#678,.F.);
#14561=ADVANCED_FACE('',(#1994),#679,.F.);
#14562=ADVANCED_FACE('',(#1995),#680,.F.);
#14563=ADVANCED_FACE('',(#1996),#681,.T.);
#14564=ADVANCED_FACE('',(#1997),#682,.T.);
#14565=ADVANCED_FACE('',(#1998),#14138,.T.);
#14566=ADVANCED_FACE('',(#1999),#683,.F.);
#14567=ADVANCED_FACE('',(#2000),#684,.F.);
#14568=ADVANCED_FACE('',(#2001),#685,.F.);
#14569=ADVANCED_FACE('',(#2002),#686,.T.);
#14570=ADVANCED_FACE('',(#2003),#687,.F.);
#14571=ADVANCED_FACE('',(#2004),#688,.T.);
#14572=ADVANCED_FACE('',(#2005),#14139,.T.);
#14573=ADVANCED_FACE('',(#2006),#689,.F.);
#14574=ADVANCED_FACE('',(#2007),#14140,.T.);
#14575=ADVANCED_FACE('',(#2008),#1489,.T.);
#14576=ADVANCED_FACE('',(#2009),#690,.T.);
#14577=ADVANCED_FACE('',(#2010),#691,.T.);
#14578=ADVANCED_FACE('',(#2011),#14141,.T.);
#14579=ADVANCED_FACE('',(#2012),#692,.F.);
#14580=ADVANCED_FACE('',(#2013),#693,.F.);
#14581=ADVANCED_FACE('',(#2014),#694,.F.);
#14582=ADVANCED_FACE('',(#2015),#695,.T.);
#14583=ADVANCED_FACE('',(#2016),#696,.T.);
#14584=ADVANCED_FACE('',(#2017),#14142,.T.);
#14585=ADVANCED_FACE('',(#2018),#697,.F.);
#14586=ADVANCED_FACE('',(#2019),#698,.F.);
#14587=ADVANCED_FACE('',(#2020),#699,.F.);
#14588=ADVANCED_FACE('',(#2021),#700,.T.);
#14589=ADVANCED_FACE('',(#2022),#701,.F.);
#14590=ADVANCED_FACE('',(#2023),#702,.T.);
#14591=ADVANCED_FACE('',(#2024),#703,.F.);
#14592=ADVANCED_FACE('',(#2025),#704,.T.);
#14593=ADVANCED_FACE('',(#2026),#705,.F.);
#14594=ADVANCED_FACE('',(#2027),#706,.T.);
#14595=ADVANCED_FACE('',(#2028),#707,.F.);
#14596=ADVANCED_FACE('',(#2029),#708,.T.);
#14597=ADVANCED_FACE('',(#2030),#709,.F.);
#14598=ADVANCED_FACE('',(#2031),#710,.T.);
#14599=ADVANCED_FACE('',(#2032),#711,.F.);
#14600=ADVANCED_FACE('',(#2033),#712,.T.);
#14601=ADVANCED_FACE('',(#2034),#713,.F.);
#14602=ADVANCED_FACE('',(#2035),#714,.T.);
#14603=ADVANCED_FACE('',(#2036),#715,.F.);
#14604=ADVANCED_FACE('',(#2037),#716,.T.);
#14605=ADVANCED_FACE('',(#2038),#717,.F.);
#14606=ADVANCED_FACE('',(#2039),#718,.T.);
#14607=ADVANCED_FACE('',(#2040),#719,.F.);
#14608=ADVANCED_FACE('',(#2041),#720,.T.);
#14609=ADVANCED_FACE('',(#2042),#721,.F.);
#14610=ADVANCED_FACE('',(#2043),#722,.T.);
#14611=ADVANCED_FACE('',(#2044),#723,.F.);
#14612=ADVANCED_FACE('',(#2045),#724,.T.);
#14613=ADVANCED_FACE('',(#2046),#725,.T.);
#14614=ADVANCED_FACE('',(#2047),#14143,.T.);
#14615=ADVANCED_FACE('',(#2048),#726,.F.);
#14616=ADVANCED_FACE('',(#2049),#727,.F.);
#14617=ADVANCED_FACE('',(#2050),#728,.F.);
#14618=ADVANCED_FACE('',(#2051),#729,.T.);
#14619=ADVANCED_FACE('',(#2052),#730,.T.);
#14620=ADVANCED_FACE('',(#2053),#14144,.T.);
#14621=ADVANCED_FACE('',(#2054),#731,.F.);
#14622=ADVANCED_FACE('',(#2055),#732,.F.);
#14623=ADVANCED_FACE('',(#2056),#733,.F.);
#14624=ADVANCED_FACE('',(#2057),#734,.T.);
#14625=ADVANCED_FACE('',(#2058),#735,.T.);
#14626=ADVANCED_FACE('',(#2059),#14145,.T.);
#14627=ADVANCED_FACE('',(#2060),#736,.F.);
#14628=ADVANCED_FACE('',(#2061),#737,.F.);
#14629=ADVANCED_FACE('',(#2062),#738,.F.);
#14630=ADVANCED_FACE('',(#2063),#739,.T.);
#14631=ADVANCED_FACE('',(#2064),#740,.T.);
#14632=ADVANCED_FACE('',(#2065),#14146,.T.);
#14633=ADVANCED_FACE('',(#2066),#741,.F.);
#14634=ADVANCED_FACE('',(#2067),#742,.F.);
#14635=ADVANCED_FACE('',(#2068),#743,.F.);
#14636=ADVANCED_FACE('',(#2069),#744,.T.);
#14637=ADVANCED_FACE('',(#2070),#745,.T.);
#14638=ADVANCED_FACE('',(#2071),#14147,.T.);
#14639=ADVANCED_FACE('',(#2072),#746,.F.);
#14640=ADVANCED_FACE('',(#2073),#747,.F.);
#14641=ADVANCED_FACE('',(#2074),#14148,.T.);
#14642=ADVANCED_FACE('',(#2075),#748,.T.);
#14643=ADVANCED_FACE('',(#2076),#749,.F.);
#14644=ADVANCED_FACE('',(#2077),#750,.T.);
#14645=ADVANCED_FACE('',(#2078),#751,.T.);
#14646=ADVANCED_FACE('',(#2079),#14149,.T.);
#14647=ADVANCED_FACE('',(#2080),#752,.F.);
#14648=ADVANCED_FACE('',(#2081),#753,.F.);
#14649=ADVANCED_FACE('',(#2082),#14150,.T.);
#14650=ADVANCED_FACE('',(#2083),#14151,.F.);
#14651=ADVANCED_FACE('',(#2084),#1490,.F.);
#14652=ADVANCED_FACE('',(#2085,#486),#754,.T.);
#14653=ADVANCED_FACE('',(#2086),#755,.F.);
#14654=ADVANCED_FACE('',(#2087),#756,.F.);
#14655=ADVANCED_FACE('',(#2088),#757,.F.);
#14656=ADVANCED_FACE('',(#2089),#758,.F.);
#14657=ADVANCED_FACE('',(#2090),#759,.F.);
#14658=ADVANCED_FACE('',(#2091),#760,.F.);
#14659=ADVANCED_FACE('',(#2092),#761,.F.);
#14660=ADVANCED_FACE('',(#2093),#14152,.T.);
#14661=ADVANCED_FACE('',(#2094),#14153,.T.);
#14662=ADVANCED_FACE('',(#2095),#14154,.T.);
#14663=ADVANCED_FACE('',(#2096),#14155,.T.);
#14664=ADVANCED_FACE('',(#2097),#762,.F.);
#14665=ADVANCED_FACE('',(#2098),#14156,.T.);
#14666=ADVANCED_FACE('',(#2099),#14157,.T.);
#14667=ADVANCED_FACE('',(#2100),#14158,.T.);
#14668=ADVANCED_FACE('',(#2101),#14159,.T.);
#14669=ADVANCED_FACE('',(#2102),#14160,.T.);
#14670=ADVANCED_FACE('',(#2103),#763,.F.);
#14671=ADVANCED_FACE('',(#2104),#14161,.T.);
#14672=ADVANCED_FACE('',(#2105,#487),#764,.T.);
#14673=ADVANCED_FACE('',(#2106),#1491,.T.);
#14674=ADVANCED_FACE('',(#2107,#488),#765,.T.);
#14675=ADVANCED_FACE('',(#2108),#1492,.T.);
#14676=ADVANCED_FACE('',(#2109,#489),#766,.T.);
#14677=ADVANCED_FACE('',(#2110,#490),#1493,.T.);
#14678=ADVANCED_FACE('',(#2111),#14162,.T.);
#14679=ADVANCED_FACE('',(#2112),#767,.T.);
#14680=ADVANCED_FACE('',(#2113),#768,.T.);
#14681=ADVANCED_FACE('',(#2114),#769,.T.);
#14682=ADVANCED_FACE('',(#2115),#770,.T.);
#14683=ADVANCED_FACE('',(#2116),#771,.T.);
#14684=ADVANCED_FACE('',(#2117),#772,.T.);
#14685=ADVANCED_FACE('',(#2118),#773,.T.);
#14686=ADVANCED_FACE('',(#2119),#774,.T.);
#14687=ADVANCED_FACE('',(#2120),#775,.T.);
#14688=ADVANCED_FACE('',(#2121),#776,.T.);
#14689=ADVANCED_FACE('',(#2122),#777,.T.);
#14690=ADVANCED_FACE('',(#2123),#778,.T.);
#14691=ADVANCED_FACE('',(#2124),#779,.T.);
#14692=ADVANCED_FACE('',(#2125),#780,.T.);
#14693=ADVANCED_FACE('',(#2126),#781,.T.);
#14694=ADVANCED_FACE('',(#2127),#782,.T.);
#14695=ADVANCED_FACE('',(#2128),#783,.T.);
#14696=ADVANCED_FACE('',(#2129),#784,.T.);
#14697=ADVANCED_FACE('',(#2130),#785,.F.);
#14698=ADVANCED_FACE('',(#2131),#14163,.T.);
#14699=ADVANCED_FACE('',(#2132,#491),#786,.T.);
#14700=ADVANCED_FACE('',(#2133),#14164,.F.);
#14701=ADVANCED_FACE('',(#2134,#492),#787,.T.);
#14702=ADVANCED_FACE('',(#2135),#14165,.T.);
#14703=ADVANCED_FACE('',(#2136),#1494,.T.);
#14704=ADVANCED_FACE('',(#2137),#14166,.T.);
#14705=ADVANCED_FACE('',(#2138,#493),#788,.T.);
#14706=ADVANCED_FACE('',(#2139),#14167,.F.);
#14707=ADVANCED_FACE('',(#2140,#494),#789,.T.);
#14708=ADVANCED_FACE('',(#2141),#14168,.T.);
#14709=ADVANCED_FACE('',(#2142,#495),#790,.T.);
#14710=ADVANCED_FACE('',(#2143),#14169,.F.);
#14711=ADVANCED_FACE('',(#2144),#1495,.F.);
#14712=ADVANCED_FACE('',(#2145),#14170,.F.);
#14713=ADVANCED_FACE('',(#2146,#496),#791,.T.);
#14714=ADVANCED_FACE('',(#2147),#1496,.F.);
#14715=ADVANCED_FACE('',(#2148,#497),#792,.T.);
#14716=ADVANCED_FACE('',(#2149,#498),#793,.T.);
#14717=ADVANCED_FACE('',(#2150),#1497,.F.);
#14718=ADVANCED_FACE('',(#2151),#1498,.F.);
#14719=ADVANCED_FACE('',(#2152,#499),#794,.T.);
#14720=ADVANCED_FACE('',(#2153),#1499,.T.);
#14721=ADVANCED_FACE('',(#2154,#500),#795,.T.);
#14722=ADVANCED_FACE('',(#2155),#1500,.F.);
#14723=ADVANCED_FACE('',(#2156,#501),#796,.T.);
#14724=ADVANCED_FACE('',(#2157),#1501,.F.);
#14725=ADVANCED_FACE('',(#2158,#502),#797,.T.);
#14726=ADVANCED_FACE('',(#2159),#14171,.F.);
#14727=ADVANCED_FACE('',(#2160,#503),#798,.T.);
#14728=ADVANCED_FACE('',(#2161),#1502,.F.);
#14729=ADVANCED_FACE('',(#2162),#14172,.T.);
#14730=ADVANCED_FACE('',(#2163,#504),#799,.T.);
#14731=ADVANCED_FACE('',(#2164),#14173,.T.);
#14732=ADVANCED_FACE('',(#2165),#1503,.F.);
#14733=ADVANCED_FACE('',(#2166,#505),#800,.T.);
#14734=ADVANCED_FACE('',(#2167),#1504,.T.);
#14735=ADVANCED_FACE('',(#2168,#506),#801,.T.);
#14736=ADVANCED_FACE('',(#2169),#14174,.F.);
#14737=ADVANCED_FACE('',(#2170),#14175,.F.);
#14738=ADVANCED_FACE('',(#2171),#1505,.F.);
#14739=ADVANCED_FACE('',(#2172,#507),#802,.T.);
#14740=ADVANCED_FACE('',(#2173),#1506,.F.);
#14741=ADVANCED_FACE('',(#2174,#508),#803,.F.);
#14742=ADVANCED_FACE('',(#2175),#1507,.T.);
#14743=ADVANCED_FACE('',(#2176,#509),#804,.T.);
#14744=ADVANCED_FACE('',(#2177),#14176,.T.);
#14745=ADVANCED_FACE('',(#2178),#1508,.T.);
#14746=ADVANCED_FACE('',(#2179),#14177,.T.);
#14747=ADVANCED_FACE('',(#2180),#131,.F.);
#14748=ADVANCED_FACE('',(#2181),#1509,.F.);
#14749=ADVANCED_FACE('',(#2182,#510),#805,.T.);
#14750=ADVANCED_FACE('',(#2183),#14178,.T.);
#14751=ADVANCED_FACE('',(#2184),#1510,.T.);
#14752=ADVANCED_FACE('',(#2185,#511),#806,.T.);
#14753=ADVANCED_FACE('',(#2186),#1511,.T.);
#14754=ADVANCED_FACE('',(#2187,#512),#807,.T.);
#14755=ADVANCED_FACE('',(#2188,#513),#146,.F.);
#14756=ADVANCED_FACE('',(#2189),#1512,.F.);
#14757=ADVANCED_FACE('',(#2190,#514),#808,.T.);
#14758=ADVANCED_FACE('',(#2191),#14179,.T.);
#14759=ADVANCED_FACE('',(#2192,#515),#809,.T.);
#14760=ADVANCED_FACE('',(#2193),#1513,.T.);
#14761=ADVANCED_FACE('',(#2194),#1514,.F.);
#14762=ADVANCED_FACE('',(#2195),#1515,.F.);
#14763=ADVANCED_FACE('',(#2196),#1516,.F.);
#14764=ADVANCED_FACE('',(#2197),#1517,.F.);
#14765=ADVANCED_FACE('',(#2198),#1518,.F.);
#14766=ADVANCED_FACE('',(#2199),#1519,.F.);
#14767=ADVANCED_FACE('',(#2200),#1520,.F.);
#14768=ADVANCED_FACE('',(#2201),#1521,.F.);
#14769=ADVANCED_FACE('',(#2202),#1522,.F.);
#14770=ADVANCED_FACE('',(#2203),#1523,.F.);
#14771=ADVANCED_FACE('',(#2204),#1524,.F.);
#14772=ADVANCED_FACE('',(#2205),#1525,.F.);
#14773=ADVANCED_FACE('',(#2206),#1526,.F.);
#14774=ADVANCED_FACE('',(#2207,#516),#810,.T.);
#14775=ADVANCED_FACE('',(#2208),#1527,.F.);
#14776=ADVANCED_FACE('',(#2209),#14180,.T.);
#14777=ADVANCED_FACE('',(#2210),#1528,.T.);
#14778=ADVANCED_FACE('',(#2211),#1529,.T.);
#14779=ADVANCED_FACE('',(#2212),#1530,.T.);
#14780=ADVANCED_FACE('',(#2213),#1531,.T.);
#14781=ADVANCED_FACE('',(#2214),#1532,.T.);
#14782=ADVANCED_FACE('',(#2215),#1533,.T.);
#14783=ADVANCED_FACE('',(#2216),#1534,.T.);
#14784=ADVANCED_FACE('',(#2217),#1535,.T.);
#14785=ADVANCED_FACE('',(#2218),#1536,.T.);
#14786=ADVANCED_FACE('',(#2219),#1537,.T.);
#14787=ADVANCED_FACE('',(#2220),#1538,.T.);
#14788=ADVANCED_FACE('',(#2221),#1539,.T.);
#14789=ADVANCED_FACE('',(#2222),#1540,.T.);
#14790=ADVANCED_FACE('',(#2223),#1541,.T.);
#14791=ADVANCED_FACE('',(#2224),#1542,.T.);
#14792=ADVANCED_FACE('',(#2225),#1543,.T.);
#14793=ADVANCED_FACE('',(#2226),#1544,.T.);
#14794=ADVANCED_FACE('',(#2227),#1545,.T.);
#14795=ADVANCED_FACE('',(#2228),#1546,.T.);
#14796=ADVANCED_FACE('',(#2229),#1547,.T.);
#14797=ADVANCED_FACE('',(#2230),#1548,.T.);
#14798=ADVANCED_FACE('',(#2231),#1549,.T.);
#14799=ADVANCED_FACE('',(#2232),#1550,.T.);
#14800=ADVANCED_FACE('',(#2233),#1551,.T.);
#14801=ADVANCED_FACE('',(#2234),#1552,.T.);
#14802=ADVANCED_FACE('',(#2235),#1553,.T.);
#14803=ADVANCED_FACE('',(#2236),#1554,.T.);
#14804=ADVANCED_FACE('',(#2237),#1555,.T.);
#14805=ADVANCED_FACE('',(#2238),#1556,.T.);
#14806=ADVANCED_FACE('',(#2239),#1557,.T.);
#14807=ADVANCED_FACE('',(#2240),#1558,.T.);
#14808=ADVANCED_FACE('',(#2241),#1559,.T.);
#14809=ADVANCED_FACE('',(#2242),#1560,.T.);
#14810=ADVANCED_FACE('',(#2243),#1561,.T.);
#14811=ADVANCED_FACE('',(#2244),#1562,.T.);
#14812=ADVANCED_FACE('',(#2245),#1563,.T.);
#14813=ADVANCED_FACE('',(#2246),#1564,.T.);
#14814=ADVANCED_FACE('',(#2247),#1565,.T.);
#14815=ADVANCED_FACE('',(#2248),#1566,.T.);
#14816=ADVANCED_FACE('',(#2249),#1567,.T.);
#14817=ADVANCED_FACE('',(#2250),#1568,.T.);
#14818=ADVANCED_FACE('',(#2251),#1569,.T.);
#14819=ADVANCED_FACE('',(#2252),#1570,.T.);
#14820=ADVANCED_FACE('',(#2253),#1571,.T.);
#14821=ADVANCED_FACE('',(#2254),#1572,.T.);
#14822=ADVANCED_FACE('',(#2255),#1573,.T.);
#14823=ADVANCED_FACE('',(#2256),#1574,.T.);
#14824=ADVANCED_FACE('',(#2257),#1575,.T.);
#14825=ADVANCED_FACE('',(#2258),#1576,.T.);
#14826=ADVANCED_FACE('',(#2259),#1577,.T.);
#14827=ADVANCED_FACE('',(#2260),#1578,.T.);
#14828=ADVANCED_FACE('',(#2261),#1579,.T.);
#14829=ADVANCED_FACE('',(#2262),#1580,.T.);
#14830=ADVANCED_FACE('',(#2263),#1581,.T.);
#14831=ADVANCED_FACE('',(#2264),#1582,.T.);
#14832=ADVANCED_FACE('',(#2265),#1583,.T.);
#14833=ADVANCED_FACE('',(#2266),#1584,.T.);
#14834=ADVANCED_FACE('',(#2267),#1585,.T.);
#14835=ADVANCED_FACE('',(#2268),#1586,.T.);
#14836=ADVANCED_FACE('',(#2269),#1587,.T.);
#14837=ADVANCED_FACE('',(#2270),#1588,.T.);
#14838=ADVANCED_FACE('',(#2271),#1589,.T.);
#14839=ADVANCED_FACE('',(#2272),#1590,.T.);
#14840=ADVANCED_FACE('',(#2273),#1591,.T.);
#14841=ADVANCED_FACE('',(#2274),#1592,.T.);
#14842=ADVANCED_FACE('',(#2275),#1593,.T.);
#14843=ADVANCED_FACE('',(#2276),#1594,.T.);
#14844=ADVANCED_FACE('',(#2277),#1595,.T.);
#14845=ADVANCED_FACE('',(#2278),#252,.F.);
#14846=ADVANCED_FACE('',(#2279),#811,.T.);
#14847=ADVANCED_FACE('',(#2280),#1596,.T.);
#14848=ADVANCED_FACE('',(#2281),#253,.F.);
#14849=ADVANCED_FACE('',(#2282),#812,.F.);
#14850=ADVANCED_FACE('',(#2283),#813,.T.);
#14851=ADVANCED_FACE('',(#2284),#814,.F.);
#14852=ADVANCED_FACE('',(#2285),#815,.F.);
#14853=ADVANCED_FACE('',(#2286),#816,.F.);
#14854=ADVANCED_FACE('',(#2287),#817,.T.);
#14855=ADVANCED_FACE('',(#2288),#818,.F.);
#14856=ADVANCED_FACE('',(#2289),#819,.F.);
#14857=ADVANCED_FACE('',(#2290),#820,.F.);
#14858=ADVANCED_FACE('',(#2291),#821,.T.);
#14859=ADVANCED_FACE('',(#2292),#822,.F.);
#14860=ADVANCED_FACE('',(#2293),#823,.F.);
#14861=ADVANCED_FACE('',(#2294),#824,.F.);
#14862=ADVANCED_FACE('',(#2295),#825,.T.);
#14863=ADVANCED_FACE('',(#2296),#826,.F.);
#14864=ADVANCED_FACE('',(#2297),#827,.F.);
#14865=ADVANCED_FACE('',(#2298),#828,.F.);
#14866=ADVANCED_FACE('',(#2299),#829,.T.);
#14867=ADVANCED_FACE('',(#2300),#830,.F.);
#14868=ADVANCED_FACE('',(#2301),#831,.F.);
#14869=ADVANCED_FACE('',(#2302),#832,.F.);
#14870=ADVANCED_FACE('',(#2303),#833,.T.);
#14871=ADVANCED_FACE('',(#2304),#834,.F.);
#14872=ADVANCED_FACE('',(#2305),#835,.F.);
#14873=ADVANCED_FACE('',(#2306),#836,.F.);
#14874=ADVANCED_FACE('',(#2307),#837,.T.);
#14875=ADVANCED_FACE('',(#2308),#838,.F.);
#14876=ADVANCED_FACE('',(#2309),#839,.F.);
#14877=ADVANCED_FACE('',(#2310),#840,.F.);
#14878=ADVANCED_FACE('',(#2311),#841,.T.);
#14879=ADVANCED_FACE('',(#2312),#842,.F.);
#14880=ADVANCED_FACE('',(#2313),#843,.F.);
#14881=ADVANCED_FACE('',(#2314),#844,.F.);
#14882=ADVANCED_FACE('',(#2315),#845,.T.);
#14883=ADVANCED_FACE('',(#2316),#846,.F.);
#14884=ADVANCED_FACE('',(#2317),#847,.F.);
#14885=ADVANCED_FACE('',(#2318),#848,.F.);
#14886=ADVANCED_FACE('',(#2319),#849,.T.);
#14887=ADVANCED_FACE('',(#2320),#850,.F.);
#14888=ADVANCED_FACE('',(#2321),#851,.F.);
#14889=ADVANCED_FACE('',(#2322),#852,.F.);
#14890=ADVANCED_FACE('',(#2323),#853,.T.);
#14891=ADVANCED_FACE('',(#2324),#854,.F.);
#14892=ADVANCED_FACE('',(#2325),#855,.F.);
#14893=ADVANCED_FACE('',(#2326),#856,.F.);
#14894=ADVANCED_FACE('',(#2327),#857,.T.);
#14895=ADVANCED_FACE('',(#2328),#858,.F.);
#14896=ADVANCED_FACE('',(#2329),#859,.F.);
#14897=ADVANCED_FACE('',(#2330),#860,.F.);
#14898=ADVANCED_FACE('',(#2331),#861,.T.);
#14899=ADVANCED_FACE('',(#2332),#862,.F.);
#14900=ADVANCED_FACE('',(#2333),#863,.F.);
#14901=ADVANCED_FACE('',(#2334),#864,.F.);
#14902=ADVANCED_FACE('',(#2335),#865,.T.);
#14903=ADVANCED_FACE('',(#2336),#866,.F.);
#14904=ADVANCED_FACE('',(#2337),#867,.F.);
#14905=ADVANCED_FACE('',(#2338),#868,.F.);
#14906=ADVANCED_FACE('',(#2339),#869,.T.);
#14907=ADVANCED_FACE('',(#2340),#870,.F.);
#14908=ADVANCED_FACE('',(#2341),#871,.F.);
#14909=ADVANCED_FACE('',(#2342),#872,.F.);
#14910=ADVANCED_FACE('',(#2343),#873,.T.);
#14911=ADVANCED_FACE('',(#2344),#874,.F.);
#14912=ADVANCED_FACE('',(#2345),#875,.F.);
#14913=ADVANCED_FACE('',(#2346),#876,.F.);
#14914=ADVANCED_FACE('',(#2347),#877,.T.);
#14915=ADVANCED_FACE('',(#2348),#878,.F.);
#14916=ADVANCED_FACE('',(#2349),#879,.F.);
#14917=ADVANCED_FACE('',(#2350),#880,.F.);
#14918=ADVANCED_FACE('',(#2351),#881,.T.);
#14919=ADVANCED_FACE('',(#2352),#882,.F.);
#14920=ADVANCED_FACE('',(#2353),#883,.F.);
#14921=ADVANCED_FACE('',(#2354),#884,.F.);
#14922=ADVANCED_FACE('',(#2355),#885,.T.);
#14923=ADVANCED_FACE('',(#2356),#886,.F.);
#14924=ADVANCED_FACE('',(#2357),#887,.F.);
#14925=ADVANCED_FACE('',(#2358),#888,.F.);
#14926=ADVANCED_FACE('',(#2359),#889,.T.);
#14927=ADVANCED_FACE('',(#2360),#890,.F.);
#14928=ADVANCED_FACE('',(#2361),#891,.F.);
#14929=ADVANCED_FACE('',(#2362),#892,.F.);
#14930=ADVANCED_FACE('',(#2363),#893,.T.);
#14931=ADVANCED_FACE('',(#2364),#894,.F.);
#14932=ADVANCED_FACE('',(#2365),#895,.F.);
#14933=ADVANCED_FACE('',(#2366),#896,.F.);
#14934=ADVANCED_FACE('',(#2367),#897,.T.);
#14935=ADVANCED_FACE('',(#2368),#898,.F.);
#14936=ADVANCED_FACE('',(#2369),#899,.F.);
#14937=ADVANCED_FACE('',(#2370),#900,.F.);
#14938=ADVANCED_FACE('',(#2371),#901,.T.);
#14939=ADVANCED_FACE('',(#2372),#902,.F.);
#14940=ADVANCED_FACE('',(#2373),#903,.F.);
#14941=ADVANCED_FACE('',(#2374),#904,.F.);
#14942=ADVANCED_FACE('',(#2375),#905,.T.);
#14943=ADVANCED_FACE('',(#2376),#906,.F.);
#14944=ADVANCED_FACE('',(#2377),#907,.F.);
#14945=ADVANCED_FACE('',(#2378),#908,.F.);
#14946=ADVANCED_FACE('',(#2379),#909,.T.);
#14947=ADVANCED_FACE('',(#2380),#910,.F.);
#14948=ADVANCED_FACE('',(#2381),#911,.F.);
#14949=ADVANCED_FACE('',(#2382),#912,.F.);
#14950=ADVANCED_FACE('',(#2383),#913,.T.);
#14951=ADVANCED_FACE('',(#2384),#914,.F.);
#14952=ADVANCED_FACE('',(#2385),#915,.F.);
#14953=ADVANCED_FACE('',(#2386),#916,.F.);
#14954=ADVANCED_FACE('',(#2387),#917,.T.);
#14955=ADVANCED_FACE('',(#2388),#918,.F.);
#14956=ADVANCED_FACE('',(#2389),#919,.F.);
#14957=ADVANCED_FACE('',(#2390),#920,.F.);
#14958=ADVANCED_FACE('',(#2391),#921,.T.);
#14959=ADVANCED_FACE('',(#2392),#922,.F.);
#14960=ADVANCED_FACE('',(#2393),#923,.F.);
#14961=ADVANCED_FACE('',(#2394),#924,.F.);
#14962=ADVANCED_FACE('',(#2395),#925,.T.);
#14963=ADVANCED_FACE('',(#2396),#926,.F.);
#14964=ADVANCED_FACE('',(#2397),#927,.F.);
#14965=ADVANCED_FACE('',(#2398),#928,.F.);
#14966=ADVANCED_FACE('',(#2399),#929,.T.);
#14967=ADVANCED_FACE('',(#2400),#930,.F.);
#14968=ADVANCED_FACE('',(#2401),#931,.F.);
#14969=ADVANCED_FACE('',(#2402),#932,.F.);
#14970=ADVANCED_FACE('',(#2403),#933,.T.);
#14971=ADVANCED_FACE('',(#2404),#934,.F.);
#14972=ADVANCED_FACE('',(#2405),#935,.F.);
#14973=ADVANCED_FACE('',(#2406),#936,.F.);
#14974=ADVANCED_FACE('',(#2407),#937,.T.);
#14975=ADVANCED_FACE('',(#2408),#938,.F.);
#14976=ADVANCED_FACE('',(#2409),#939,.F.);
#14977=ADVANCED_FACE('',(#2410),#940,.F.);
#14978=ADVANCED_FACE('',(#2411),#941,.T.);
#14979=ADVANCED_FACE('',(#2412),#942,.F.);
#14980=ADVANCED_FACE('',(#2413),#943,.F.);
#14981=ADVANCED_FACE('',(#2414),#944,.F.);
#14982=ADVANCED_FACE('',(#2415),#945,.T.);
#14983=ADVANCED_FACE('',(#2416),#946,.F.);
#14984=ADVANCED_FACE('',(#2417),#947,.F.);
#14985=ADVANCED_FACE('',(#2418),#948,.F.);
#14986=ADVANCED_FACE('',(#2419),#949,.T.);
#14987=ADVANCED_FACE('',(#2420),#950,.F.);
#14988=ADVANCED_FACE('',(#2421),#951,.F.);
#14989=ADVANCED_FACE('',(#2422),#952,.F.);
#14990=ADVANCED_FACE('',(#2423),#953,.T.);
#14991=ADVANCED_FACE('',(#2424),#954,.F.);
#14992=ADVANCED_FACE('',(#2425),#955,.F.);
#14993=ADVANCED_FACE('',(#2426),#956,.F.);
#14994=ADVANCED_FACE('',(#2427),#957,.F.);
#14995=ADVANCED_FACE('',(#2428),#958,.F.);
#14996=ADVANCED_FACE('',(#2429),#959,.F.);
#14997=ADVANCED_FACE('',(#2430),#960,.F.);
#14998=ADVANCED_FACE('',(#2431),#961,.F.);
#14999=ADVANCED_FACE('',(#2432),#962,.F.);
#15000=ADVANCED_FACE('',(#2433),#963,.T.);
#15001=ADVANCED_FACE('',(#2434),#14181,.T.);
#15002=ADVANCED_FACE('',(#2435),#1597,.T.);
#15003=ADVANCED_FACE('',(#2436,#517),#964,.T.);
#15004=ADVANCED_FACE('',(#2437,#518,#519,#520,#521,#522,#523,#524,#525,
#526,#527,#528,#529,#530,#531,#532,#533,#534,#535,#536,#537,#538,#539,#540,
#541,#542,#543,#544,#545,#546,#547,#548,#549,#550,#551,#552),#1598,.T.);
#15005=ADVANCED_FACE('',(#2438),#14182,.T.);
#15006=ADVANCED_FACE('',(#2439,#553),#965,.T.);
#15007=ADVANCED_FACE('',(#2440),#1599,.T.);
#15008=ADVANCED_FACE('',(#2441),#1600,.T.);
#15009=ADVANCED_FACE('',(#2442),#1601,.T.);
#15010=ADVANCED_FACE('',(#2443),#1602,.T.);
#15011=ADVANCED_FACE('',(#2444),#1603,.T.);
#15012=ADVANCED_FACE('',(#2445),#1604,.T.);
#15013=ADVANCED_FACE('',(#2446),#1605,.T.);
#15014=ADVANCED_FACE('',(#2447),#1606,.T.);
#15015=ADVANCED_FACE('',(#2448),#1607,.T.);
#15016=ADVANCED_FACE('',(#2449),#1608,.T.);
#15017=ADVANCED_FACE('',(#2450),#1609,.T.);
#15018=ADVANCED_FACE('',(#2451),#1610,.T.);
#15019=ADVANCED_FACE('',(#2452),#1611,.T.);
#15020=ADVANCED_FACE('',(#2453),#1612,.T.);
#15021=ADVANCED_FACE('',(#2454),#966,.T.);
#15022=ADVANCED_FACE('',(#2455),#967,.T.);
#15023=ADVANCED_FACE('',(#2456),#968,.T.);
#15024=ADVANCED_FACE('',(#2457),#969,.T.);
#15025=ADVANCED_FACE('',(#2458),#970,.T.);
#15026=ADVANCED_FACE('',(#2459),#971,.T.);
#15027=ADVANCED_FACE('',(#2460),#972,.T.);
#15028=ADVANCED_FACE('',(#2461),#973,.T.);
#15029=ADVANCED_FACE('',(#2462),#974,.T.);
#15030=ADVANCED_FACE('',(#2463),#975,.T.);
#15031=ADVANCED_FACE('',(#2464),#976,.T.);
#15032=ADVANCED_FACE('',(#2465),#977,.T.);
#15033=ADVANCED_FACE('',(#2466),#978,.T.);
#15034=ADVANCED_FACE('',(#2467),#979,.T.);
#15035=ADVANCED_FACE('',(#2468),#980,.T.);
#15036=ADVANCED_FACE('',(#2469),#981,.T.);
#15037=ADVANCED_FACE('',(#2470),#982,.T.);
#15038=ADVANCED_FACE('',(#2471),#983,.T.);
#15039=ADVANCED_FACE('',(#2472),#984,.T.);
#15040=ADVANCED_FACE('',(#2473),#985,.T.);
#15041=ADVANCED_FACE('',(#2474),#986,.T.);
#15042=ADVANCED_FACE('',(#2475,#554),#987,.T.);
#15043=ADVANCED_FACE('',(#2476),#988,.T.);
#15044=ADVANCED_FACE('',(#2477),#989,.T.);
#15045=ADVANCED_FACE('',(#2478),#990,.T.);
#15046=ADVANCED_FACE('',(#2479),#991,.T.);
#15047=ADVANCED_FACE('',(#2480),#992,.T.);
#15048=ADVANCED_FACE('',(#2481),#993,.T.);
#15049=ADVANCED_FACE('',(#2482),#994,.F.);
#15050=ADVANCED_FACE('',(#2483),#995,.F.);
#15051=ADVANCED_FACE('',(#2484),#996,.F.);
#15052=ADVANCED_FACE('',(#2485),#254,.F.);
#15053=ADVANCED_FACE('',(#2486),#997,.T.);
#15054=ADVANCED_FACE('',(#2487),#1613,.T.);
#15055=ADVANCED_FACE('',(#2488),#255,.F.);
#15056=ADVANCED_FACE('',(#2489,#555),#998,.T.);
#15057=ADVANCED_FACE('',(#2490),#999,.F.);
#15058=ADVANCED_FACE('',(#2491),#1000,.F.);
#15059=ADVANCED_FACE('',(#2492),#1001,.F.);
#15060=ADVANCED_FACE('',(#2493),#1002,.F.);
#15061=ADVANCED_FACE('',(#2494),#1003,.T.);
#15062=ADVANCED_FACE('',(#2495),#1004,.T.);
#15063=ADVANCED_FACE('',(#2496),#1005,.T.);
#15064=ADVANCED_FACE('',(#2497,#556),#1006,.T.);
#15065=ADVANCED_FACE('',(#2498,#557),#1007,.T.);
#15066=ADVANCED_FACE('',(#2499),#1614,.T.);
#15067=ADVANCED_FACE('',(#2500),#1008,.T.);
#15068=ADVANCED_FACE('',(#2501),#14183,.T.);
#15069=ADVANCED_FACE('',(#2502),#1615,.T.);
#15070=ADVANCED_FACE('',(#2503),#1616,.T.);
#15071=CLOSED_SHELL('',(#14184,#14185,#14186,#14187,#14188,#14189,#14190,
#14191,#14192,#14193,#14194,#14195,#14196,#14197,#14198,#14199,#14200,#14201,
#14202,#14203,#14204,#14205,#14206,#14207,#14208,#14209,#14210,#14211,#14212,
#14213,#14214,#14215,#14216,#14217,#14218,#14219,#14220,#14221,#14222,#14223,
#14224,#14225,#14226,#14227,#14228,#14229,#14230,#14231,#14232,#14233,#14234,
#14235,#14236,#14237,#14238,#14239,#14240,#14241,#14242,#14243,#14244,#14245,
#14246,#14247,#14248,#14249,#14250,#14251,#14252,#14253,#14254,#14255,#14256,
#14257,#14258,#14259,#14260,#14261,#14262,#14263,#14264,#14265,#14266,#14267,
#14268,#14269,#14270,#14271,#14272,#14273,#14274,#14275,#14276,#14277,#14278,
#14279,#14280,#14281,#14282,#14283,#14284,#14285,#14286,#14287,#14288,#14289,
#14290,#14291,#14292,#14293,#14294,#14295,#14296,#14297,#14298,#14299,#14300,
#14301,#14302,#14303));
#15072=CLOSED_SHELL('',(#14304,#14305,#14306,#14307,#14308,#14309,#14310,
#14311,#14312,#14313,#14314,#14315,#14316,#14317,#14318,#14319,#14320,#14321,
#14322,#14323,#14324,#14325,#14326,#14327,#14328,#14329,#14330,#14331,#14332,
#14333,#14334,#14335,#14336,#14337,#14338,#14339,#14340,#14341,#14342,#14343,
#14344,#14345,#14346,#14347,#14348,#14349,#14350,#14351,#14352,#14353,#14354,
#14355,#14356,#14357,#14358,#14359,#14360,#14361,#14362,#14363,#14364,#14365,
#14366,#14367,#14368,#14369,#14370,#14371,#14372,#14373,#14374,#14375,#14376,
#14377,#14378,#14379,#14380,#14381,#14382,#14383,#14384,#14385,#14386,#14387,
#14388,#14389,#14390,#14391,#14392,#14393,#14394,#14395,#14396,#14397,#14398,
#14399,#14400,#14401,#14402,#14403,#14404,#14405,#14406,#14407,#14408,#14409,
#14410,#14411,#14412,#14413,#14414,#14415,#14416,#14417,#14418,#14419,#14420,
#14421,#14422,#14423,#14424,#14425,#14426,#14427,#14428,#14429,#14430,#14431,
#14432,#14433,#14434,#14435,#14436,#14437,#14438,#14439,#14440,#14441,#14442,
#14443,#14444,#14445,#14446,#14447,#14448,#14449,#14450,#14451,#14452,#14453,
#14454,#14455,#14456,#14457,#14458,#14459,#14460,#14461,#14462,#14463,#14464,
#14465,#14466,#14467,#14468,#14469,#14470,#14471,#14472,#14473,#14474,#14475,
#14476,#14477));
#15073=CLOSED_SHELL('',(#14478,#14479,#14480,#14481,#14482,#14483,#14484,
#14485,#14486,#14487,#14488));
#15074=CLOSED_SHELL('',(#14489,#14490,#14491,#14492,#14493,#14494,#14495,
#14496,#14497,#14498,#14499,#14500,#14501,#14502,#14503,#14504,#14505,#14506,
#14507,#14508,#14509,#14510,#14511,#14512,#14513,#14514,#14515,#14516,#14517,
#14518,#14519,#14520,#14521,#14522,#14523,#14524));
#15075=CLOSED_SHELL('',(#14525,#14526,#14527,#14528,#14529,#14530,#14531,
#14532,#14533,#14534,#14535,#14536,#14537,#14538,#14539,#14540,#14541,#14542,
#14543,#14544));
#15076=CLOSED_SHELL('',(#14545,#14546,#14547,#14548,#14549,#14550,#14551,
#14552,#14553,#14554,#14555,#14556,#14557,#14558,#14559,#14560,#14561,#14562,
#14563,#14564,#14565,#14566,#14567,#14568,#14569,#14570,#14571,#14572,#14573,
#14574,#14575,#14576,#14577,#14578,#14579,#14580,#14581,#14582,#14583,#14584,
#14585,#14586,#14587,#14588,#14589,#14590,#14591,#14592,#14593,#14594,#14595,
#14596,#14597,#14598,#14599,#14600,#14601,#14602,#14603,#14604,#14605,#14606,
#14607,#14608,#14609,#14610,#14611,#14612,#14613,#14614,#14615,#14616,#14617,
#14618,#14619,#14620,#14621,#14622,#14623,#14624,#14625,#14626,#14627,#14628,
#14629,#14630,#14631,#14632,#14633,#14634,#14635,#14636,#14637,#14638,#14639,
#14640,#14641,#14642,#14643,#14644,#14645,#14646,#14647,#14648,#14649,#14650,
#14651,#14652,#14653,#14654,#14655,#14656,#14657,#14658,#14659,#14660,#14661,
#14662,#14663,#14664,#14665,#14666,#14667,#14668,#14669,#14670,#14671,#14672,
#14673,#14674,#14675,#14676,#14677,#14678,#14679));
#15077=CLOSED_SHELL('',(#14680,#14681,#14682,#14683,#14684,#14685,#14686,
#14687,#14688,#14689,#14690,#14691,#14692,#14693,#14694,#14695,#14696,#14697));
#15078=CLOSED_SHELL('',(#14698,#14699,#14700,#14701,#14702,#14703,#14704,
#14705,#14706,#14707,#14708,#14709,#14710,#14711,#14712,#14713));
#15079=CLOSED_SHELL('',(#14714,#14715,#14716,#14717,#14718,#14719,#14720,
#14721,#14722,#14723,#14724,#14725));
#15080=CLOSED_SHELL('',(#14726,#14727,#14728,#14729,#14730,#14731,#14732,
#14733,#14734,#14735,#14736));
#15081=CLOSED_SHELL('',(#14737,#14738,#14739,#14740,#14741,#14742,#14743,
#14744,#14745,#14746,#14747));
#15082=CLOSED_SHELL('',(#14748,#14749,#14750,#14751,#14752,#14753,#14754,
#14755,#14756,#14757));
#15083=CLOSED_SHELL('',(#14758,#14759,#14760,#14761,#14762,#14763,#14764,
#14765,#14766,#14767,#14768,#14769,#14770,#14771,#14772,#14773,#14774,#14775,
#14776));
#15084=CLOSED_SHELL('',(#14777,#14778,#14779,#14780,#14781,#14782,#14783,
#14784,#14785,#14786,#14787,#14788,#14789,#14790,#14791,#14792,#14793,#14794,
#14795,#14796,#14797,#14798,#14799,#14800,#14801,#14802,#14803,#14804,#14805,
#14806,#14807,#14808,#14809,#14810,#14811,#14812,#14813,#14814,#14815,#14816,
#14817,#14818,#14819,#14820,#14821,#14822,#14823,#14824,#14825,#14826,#14827,
#14828,#14829,#14830,#14831,#14832,#14833,#14834,#14835,#14836,#14837,#14838,
#14839,#14840,#14841,#14842,#14843,#14844,#14845,#14846,#14847,#14848,#14849,
#14850,#14851,#14852,#14853,#14854,#14855,#14856,#14857,#14858,#14859,#14860,
#14861,#14862,#14863,#14864,#14865,#14866,#14867,#14868,#14869,#14870,#14871,
#14872,#14873,#14874,#14875,#14876,#14877,#14878,#14879,#14880,#14881,#14882,
#14883,#14884,#14885,#14886,#14887,#14888,#14889,#14890,#14891,#14892,#14893,
#14894,#14895,#14896,#14897,#14898,#14899,#14900,#14901,#14902,#14903,#14904,
#14905,#14906,#14907,#14908,#14909,#14910,#14911,#14912,#14913,#14914,#14915,
#14916,#14917,#14918,#14919,#14920,#14921,#14922,#14923,#14924,#14925,#14926,
#14927,#14928,#14929,#14930,#14931,#14932,#14933,#14934,#14935,#14936,#14937,
#14938,#14939,#14940,#14941,#14942,#14943,#14944,#14945,#14946,#14947,#14948,
#14949,#14950,#14951,#14952,#14953,#14954,#14955,#14956,#14957,#14958,#14959,
#14960,#14961,#14962,#14963,#14964,#14965,#14966,#14967,#14968,#14969,#14970,
#14971,#14972,#14973,#14974,#14975,#14976,#14977,#14978,#14979,#14980,#14981,
#14982,#14983,#14984,#14985,#14986,#14987,#14988,#14989,#14990,#14991,#14992,
#14993,#14994,#14995,#14996,#14997,#14998,#14999,#15000,#15001,#15002,#15003,
#15004,#15005,#15006));
#15085=CLOSED_SHELL('',(#15007,#15008,#15009,#15010,#15011,#15012,#15013,
#15014,#15015,#15016,#15017,#15018,#15019,#15020,#15021,#15022,#15023,#15024,
#15025,#15026,#15027,#15028,#15029,#15030,#15031,#15032,#15033,#15034,#15035,
#15036,#15037,#15038,#15039,#15040,#15041,#15042,#15043,#15044,#15045,#15046,
#15047,#15048,#15049,#15050,#15051,#15052,#15053,#15054,#15055,#15056,#15057,
#15058,#15059,#15060,#15061,#15062,#15063,#15064,#15065,#15066,#15067,#15068,
#15069,#15070));
#15086=DERIVED_UNIT_ELEMENT(#15116,1.);
#15087=DERIVED_UNIT_ELEMENT(#38509,-3.);
#15088=DERIVED_UNIT_ELEMENT(#15116,1.);
#15089=DERIVED_UNIT_ELEMENT(#38509,-3.);
#15090=DERIVED_UNIT_ELEMENT(#15116,1.);
#15091=DERIVED_UNIT_ELEMENT(#38509,-3.);
#15092=DERIVED_UNIT_ELEMENT(#15116,1.);
#15093=DERIVED_UNIT_ELEMENT(#38509,-3.);
#15094=DERIVED_UNIT_ELEMENT(#15116,1.);
#15095=DERIVED_UNIT_ELEMENT(#38509,-3.);
#15096=DERIVED_UNIT_ELEMENT(#15116,1.);
#15097=DERIVED_UNIT_ELEMENT(#38509,-3.);
#15098=DERIVED_UNIT_ELEMENT(#15116,1.);
#15099=DERIVED_UNIT_ELEMENT(#38509,-3.);
#15100=DERIVED_UNIT_ELEMENT(#15116,1.);
#15101=DERIVED_UNIT_ELEMENT(#38509,-3.);
#15102=DERIVED_UNIT_ELEMENT(#15116,1.);
#15103=DERIVED_UNIT_ELEMENT(#38509,-3.);
#15104=DERIVED_UNIT_ELEMENT(#15116,1.);
#15105=DERIVED_UNIT_ELEMENT(#38509,-3.);
#15106=DERIVED_UNIT_ELEMENT(#15116,1.);
#15107=DERIVED_UNIT_ELEMENT(#38509,-3.);
#15108=DERIVED_UNIT_ELEMENT(#15116,1.);
#15109=DERIVED_UNIT_ELEMENT(#38509,-3.);
#15110=DERIVED_UNIT_ELEMENT(#15116,1.);
#15111=DERIVED_UNIT_ELEMENT(#38509,-3.);
#15112=DERIVED_UNIT_ELEMENT(#15116,1.);
#15113=DERIVED_UNIT_ELEMENT(#38509,-3.);
#15114=DERIVED_UNIT_ELEMENT(#15116,1.);
#15115=DERIVED_UNIT_ELEMENT(#38509,-3.);
#15116=(
MASS_UNIT()
NAMED_UNIT(*)
SI_UNIT(.KILO.,.GRAM.)
);
#15117=DERIVED_UNIT((#15086,#15087));
#15118=DERIVED_UNIT((#15088,#15089));
#15119=DERIVED_UNIT((#15090,#15091));
#15120=DERIVED_UNIT((#15092,#15093));
#15121=DERIVED_UNIT((#15094,#15095));
#15122=DERIVED_UNIT((#15096,#15097));
#15123=DERIVED_UNIT((#15098,#15099));
#15124=DERIVED_UNIT((#15100,#15101));
#15125=DERIVED_UNIT((#15102,#15103));
#15126=DERIVED_UNIT((#15104,#15105));
#15127=DERIVED_UNIT((#15106,#15107));
#15128=DERIVED_UNIT((#15108,#15109));
#15129=DERIVED_UNIT((#15110,#15111));
#15130=DERIVED_UNIT((#15112,#15113));
#15131=DERIVED_UNIT((#15114,#15115));
#15132=MEASURE_REPRESENTATION_ITEM('density measure',
POSITIVE_RATIO_MEASURE(7850.),#15117);
#15133=MEASURE_REPRESENTATION_ITEM('density measure',
POSITIVE_RATIO_MEASURE(7850.),#15118);
#15134=MEASURE_REPRESENTATION_ITEM('density measure',
POSITIVE_RATIO_MEASURE(7850.),#15119);
#15135=MEASURE_REPRESENTATION_ITEM('density measure',
POSITIVE_RATIO_MEASURE(7850.),#15120);
#15136=MEASURE_REPRESENTATION_ITEM('density measure',
POSITIVE_RATIO_MEASURE(7850.),#15121);
#15137=MEASURE_REPRESENTATION_ITEM('density measure',
POSITIVE_RATIO_MEASURE(7850.),#15122);
#15138=MEASURE_REPRESENTATION_ITEM('density measure',
POSITIVE_RATIO_MEASURE(7850.),#15123);
#15139=MEASURE_REPRESENTATION_ITEM('density measure',
POSITIVE_RATIO_MEASURE(7850.),#15124);
#15140=MEASURE_REPRESENTATION_ITEM('density measure',
POSITIVE_RATIO_MEASURE(7850.),#15125);
#15141=MEASURE_REPRESENTATION_ITEM('density measure',
POSITIVE_RATIO_MEASURE(7850.),#15126);
#15142=MEASURE_REPRESENTATION_ITEM('density measure',
POSITIVE_RATIO_MEASURE(7850.),#15127);
#15143=MEASURE_REPRESENTATION_ITEM('density measure',
POSITIVE_RATIO_MEASURE(7850.),#15128);
#15144=MEASURE_REPRESENTATION_ITEM('density measure',
POSITIVE_RATIO_MEASURE(7850.),#15129);
#15145=MEASURE_REPRESENTATION_ITEM('density measure',
POSITIVE_RATIO_MEASURE(7850.),#15130);
#15146=MEASURE_REPRESENTATION_ITEM('density measure',
POSITIVE_RATIO_MEASURE(7850.),#15131);
#15147=PROPERTY_DEFINITION_REPRESENTATION(#15222,#15177);
#15148=PROPERTY_DEFINITION_REPRESENTATION(#15223,#15178);
#15149=PROPERTY_DEFINITION_REPRESENTATION(#15224,#15179);
#15150=PROPERTY_DEFINITION_REPRESENTATION(#15225,#15180);
#15151=PROPERTY_DEFINITION_REPRESENTATION(#15226,#15181);
#15152=PROPERTY_DEFINITION_REPRESENTATION(#15227,#15182);
#15153=PROPERTY_DEFINITION_REPRESENTATION(#15228,#15183);
#15154=PROPERTY_DEFINITION_REPRESENTATION(#15229,#15184);
#15155=PROPERTY_DEFINITION_REPRESENTATION(#15230,#15185);
#15156=PROPERTY_DEFINITION_REPRESENTATION(#15231,#15186);
#15157=PROPERTY_DEFINITION_REPRESENTATION(#15232,#15187);
#15158=PROPERTY_DEFINITION_REPRESENTATION(#15233,#15188);
#15159=PROPERTY_DEFINITION_REPRESENTATION(#15234,#15189);
#15160=PROPERTY_DEFINITION_REPRESENTATION(#15235,#15190);
#15161=PROPERTY_DEFINITION_REPRESENTATION(#15236,#15191);
#15162=PROPERTY_DEFINITION_REPRESENTATION(#15237,#15192);
#15163=PROPERTY_DEFINITION_REPRESENTATION(#15238,#15193);
#15164=PROPERTY_DEFINITION_REPRESENTATION(#15239,#15194);
#15165=PROPERTY_DEFINITION_REPRESENTATION(#15240,#15195);
#15166=PROPERTY_DEFINITION_REPRESENTATION(#15241,#15196);
#15167=PROPERTY_DEFINITION_REPRESENTATION(#15242,#15197);
#15168=PROPERTY_DEFINITION_REPRESENTATION(#15243,#15198);
#15169=PROPERTY_DEFINITION_REPRESENTATION(#15244,#15199);
#15170=PROPERTY_DEFINITION_REPRESENTATION(#15245,#15200);
#15171=PROPERTY_DEFINITION_REPRESENTATION(#15246,#15201);
#15172=PROPERTY_DEFINITION_REPRESENTATION(#15247,#15202);
#15173=PROPERTY_DEFINITION_REPRESENTATION(#15248,#15203);
#15174=PROPERTY_DEFINITION_REPRESENTATION(#15249,#15204);
#15175=PROPERTY_DEFINITION_REPRESENTATION(#15250,#15205);
#15176=PROPERTY_DEFINITION_REPRESENTATION(#15251,#15206);
#15177=REPRESENTATION('material name',(#15207),#38492);
#15178=REPRESENTATION('density',(#15132),#38492);
#15179=REPRESENTATION('material name',(#15208),#38493);
#15180=REPRESENTATION('density',(#15133),#38493);
#15181=REPRESENTATION('material name',(#15209),#38494);
#15182=REPRESENTATION('density',(#15134),#38494);
#15183=REPRESENTATION('material name',(#15210),#38495);
#15184=REPRESENTATION('density',(#15135),#38495);
#15185=REPRESENTATION('material name',(#15211),#38496);
#15186=REPRESENTATION('density',(#15136),#38496);
#15187=REPRESENTATION('material name',(#15212),#38497);
#15188=REPRESENTATION('density',(#15137),#38497);
#15189=REPRESENTATION('material name',(#15213),#38498);
#15190=REPRESENTATION('density',(#15138),#38498);
#15191=REPRESENTATION('material name',(#15214),#38499);
#15192=REPRESENTATION('density',(#15139),#38499);
#15193=REPRESENTATION('material name',(#15215),#38500);
#15194=REPRESENTATION('density',(#15140),#38500);
#15195=REPRESENTATION('material name',(#15216),#38501);
#15196=REPRESENTATION('density',(#15141),#38501);
#15197=REPRESENTATION('material name',(#15217),#38502);
#15198=REPRESENTATION('density',(#15142),#38502);
#15199=REPRESENTATION('material name',(#15218),#38503);
#15200=REPRESENTATION('density',(#15143),#38503);
#15201=REPRESENTATION('material name',(#15219),#38504);
#15202=REPRESENTATION('density',(#15144),#38504);
#15203=REPRESENTATION('material name',(#15220),#38505);
#15204=REPRESENTATION('density',(#15145),#38505);
#15205=REPRESENTATION('material name',(#15221),#38506);
#15206=REPRESENTATION('density',(#15146),#38506);
#15207=DESCRIPTIVE_REPRESENTATION_ITEM('Steel','Steel');
#15208=DESCRIPTIVE_REPRESENTATION_ITEM('Steel','Steel');
#15209=DESCRIPTIVE_REPRESENTATION_ITEM('Steel','Steel');
#15210=DESCRIPTIVE_REPRESENTATION_ITEM('Steel','Steel');
#15211=DESCRIPTIVE_REPRESENTATION_ITEM('Steel','Steel');
#15212=DESCRIPTIVE_REPRESENTATION_ITEM('Steel','Steel');
#15213=DESCRIPTIVE_REPRESENTATION_ITEM('Steel','Steel');
#15214=DESCRIPTIVE_REPRESENTATION_ITEM('Steel','Steel');
#15215=DESCRIPTIVE_REPRESENTATION_ITEM('Steel','Steel');
#15216=DESCRIPTIVE_REPRESENTATION_ITEM('Steel','Steel');
#15217=DESCRIPTIVE_REPRESENTATION_ITEM('Steel','Steel');
#15218=DESCRIPTIVE_REPRESENTATION_ITEM('Steel','Steel');
#15219=DESCRIPTIVE_REPRESENTATION_ITEM('Steel','Steel');
#15220=DESCRIPTIVE_REPRESENTATION_ITEM('Steel','Steel');
#15221=DESCRIPTIVE_REPRESENTATION_ITEM('Steel','Steel');
#15222=PROPERTY_DEFINITION('material property','material name',#38592);
#15223=PROPERTY_DEFINITION('material property','density of part',#38592);
#15224=PROPERTY_DEFINITION('material property','material name',#38593);
#15225=PROPERTY_DEFINITION('material property','density of part',#38593);
#15226=PROPERTY_DEFINITION('material property','material name',#38594);
#15227=PROPERTY_DEFINITION('material property','density of part',#38594);
#15228=PROPERTY_DEFINITION('material property','material name',#38595);
#15229=PROPERTY_DEFINITION('material property','density of part',#38595);
#15230=PROPERTY_DEFINITION('material property','material name',#38596);
#15231=PROPERTY_DEFINITION('material property','density of part',#38596);
#15232=PROPERTY_DEFINITION('material property','material name',#38597);
#15233=PROPERTY_DEFINITION('material property','density of part',#38597);
#15234=PROPERTY_DEFINITION('material property','material name',#38598);
#15235=PROPERTY_DEFINITION('material property','density of part',#38598);
#15236=PROPERTY_DEFINITION('material property','material name',#38599);
#15237=PROPERTY_DEFINITION('material property','density of part',#38599);
#15238=PROPERTY_DEFINITION('material property','material name',#38600);
#15239=PROPERTY_DEFINITION('material property','density of part',#38600);
#15240=PROPERTY_DEFINITION('material property','material name',#38601);
#15241=PROPERTY_DEFINITION('material property','density of part',#38601);
#15242=PROPERTY_DEFINITION('material property','material name',#38602);
#15243=PROPERTY_DEFINITION('material property','density of part',#38602);
#15244=PROPERTY_DEFINITION('material property','material name',#38603);
#15245=PROPERTY_DEFINITION('material property','density of part',#38603);
#15246=PROPERTY_DEFINITION('material property','material name',#38604);
#15247=PROPERTY_DEFINITION('material property','density of part',#38604);
#15248=PROPERTY_DEFINITION('material property','material name',#38605);
#15249=PROPERTY_DEFINITION('material property','density of part',#38605);
#15250=PROPERTY_DEFINITION('material property','material name',#38606);
#15251=PROPERTY_DEFINITION('material property','density of part',#38606);
#15252=AXIS2_PLACEMENT_3D('',#20890,#16775,#16776);
#15253=AXIS2_PLACEMENT_3D('',#20891,#16777,#16778);
#15254=AXIS2_PLACEMENT_3D('',#20892,#16779,#16780);
#15255=AXIS2_PLACEMENT_3D('',#20894,#16781,#16782);
#15256=AXIS2_PLACEMENT_3D('',#20897,#16784,#16785);
#15257=AXIS2_PLACEMENT_3D('',#20898,#16786,#16787);
#15258=AXIS2_PLACEMENT_3D('',#20902,#16789,#16790);
#15259=AXIS2_PLACEMENT_3D('',#20914,#16791,#16792);
#15260=AXIS2_PLACEMENT_3D('',#20915,#16793,#16794);
#15261=AXIS2_PLACEMENT_3D('',#20917,#16795,#16796);
#15262=AXIS2_PLACEMENT_3D('',#20918,#16797,#16798);
#15263=AXIS2_PLACEMENT_3D('',#20920,#16799,#16800);
#15264=AXIS2_PLACEMENT_3D('',#20923,#16802,#16803);
#15265=AXIS2_PLACEMENT_3D('',#20924,#16804,#16805);
#15266=AXIS2_PLACEMENT_3D('',#20929,#16807,#16808);
#15267=AXIS2_PLACEMENT_3D('',#20933,#16810,#16811);
#15268=AXIS2_PLACEMENT_3D('',#20936,#16813,#16814);
#15269=AXIS2_PLACEMENT_3D('',#20937,#16815,#16816);
#15270=AXIS2_PLACEMENT_3D('',#20939,#16817,#16818);
#15271=AXIS2_PLACEMENT_3D('',#20941,#16820,#16821);
#15272=AXIS2_PLACEMENT_3D('',#20943,#16822,#16823);
#15273=AXIS2_PLACEMENT_3D('',#20946,#16825,#16826);
#15274=AXIS2_PLACEMENT_3D('',#20947,#16827,#16828);
#15275=AXIS2_PLACEMENT_3D('',#20949,#16829,#16830);
#15276=AXIS2_PLACEMENT_3D('',#20950,#16831,#16832);
#15277=AXIS2_PLACEMENT_3D('',#20954,#16834,#16835);
#15278=AXIS2_PLACEMENT_3D('',#20966,#16836,#16837);
#15279=AXIS2_PLACEMENT_3D('',#20967,#16838,#16839);
#15280=AXIS2_PLACEMENT_3D('',#20969,#16840,#16841);
#15281=AXIS2_PLACEMENT_3D('',#20972,#16843,#16844);
#15282=AXIS2_PLACEMENT_3D('',#20973,#16845,#16846);
#15283=AXIS2_PLACEMENT_3D('',#20978,#16848,#16849);
#15284=AXIS2_PLACEMENT_3D('',#20982,#16851,#16852);
#15285=AXIS2_PLACEMENT_3D('',#20985,#16854,#16855);
#15286=AXIS2_PLACEMENT_3D('',#20986,#16856,#16857);
#15287=AXIS2_PLACEMENT_3D('',#20988,#16858,#16859);
#15288=AXIS2_PLACEMENT_3D('',#20990,#16861,#16862);
#15289=AXIS2_PLACEMENT_3D('',#20993,#16864,#16865);
#15290=AXIS2_PLACEMENT_3D('',#20994,#16866,#16867);
#15291=AXIS2_PLACEMENT_3D('',#21004,#16869,#16870);
#15292=AXIS2_PLACEMENT_3D('',#21014,#16871,#16872);
#15293=AXIS2_PLACEMENT_3D('',#21016,#16873,#16874);
#15294=AXIS2_PLACEMENT_3D('',#21019,#16876,#16877);
#15295=AXIS2_PLACEMENT_3D('',#21020,#16878,#16879);
#15296=AXIS2_PLACEMENT_3D('',#21025,#16881,#16882);
#15297=AXIS2_PLACEMENT_3D('',#21029,#16884,#16885);
#15298=AXIS2_PLACEMENT_3D('',#21033,#16887,#16888);
#15299=AXIS2_PLACEMENT_3D('',#21036,#16890,#16891);
#15300=AXIS2_PLACEMENT_3D('',#21038,#16892,#16893);
#15301=AXIS2_PLACEMENT_3D('',#21040,#16894,#16895);
#15302=AXIS2_PLACEMENT_3D('',#21042,#16896,#16897);
#15303=AXIS2_PLACEMENT_3D('',#21044,#16898,#16899);
#15304=AXIS2_PLACEMENT_3D('',#21045,#16900,#16901);
#15305=AXIS2_PLACEMENT_3D('',#21048,#16903,#16904);
#15306=AXIS2_PLACEMENT_3D('',#21049,#16905,#16906);
#15307=AXIS2_PLACEMENT_3D('',#21052,#16908,#16909);
#15308=AXIS2_PLACEMENT_3D('',#21053,#16910,#16911);
#15309=AXIS2_PLACEMENT_3D('',#21056,#16913,#16914);
#15310=AXIS2_PLACEMENT_3D('',#21057,#16915,#16916);
#15311=AXIS2_PLACEMENT_3D('',#21060,#16918,#16919);
#15312=AXIS2_PLACEMENT_3D('',#21061,#16920,#16921);
#15313=AXIS2_PLACEMENT_3D('',#21064,#16923,#16924);
#15314=AXIS2_PLACEMENT_3D('',#21065,#16925,#16926);
#15315=AXIS2_PLACEMENT_3D('',#21068,#16928,#16929);
#15316=AXIS2_PLACEMENT_3D('',#21069,#16930,#16931);
#15317=AXIS2_PLACEMENT_3D('',#21072,#16933,#16934);
#15318=AXIS2_PLACEMENT_3D('',#21073,#16935,#16936);
#15319=AXIS2_PLACEMENT_3D('',#21084,#16937,#16938);
#15320=AXIS2_PLACEMENT_3D('',#21093,#16939,#16940);
#15321=AXIS2_PLACEMENT_3D('',#21097,#16942,#16943);
#15322=AXIS2_PLACEMENT_3D('',#21099,#16945,#16946);
#15323=AXIS2_PLACEMENT_3D('',#21115,#16953,#16954);
#15324=AXIS2_PLACEMENT_3D('',#21131,#16956,#16957);
#15325=AXIS2_PLACEMENT_3D('',#21133,#16959,#16960);
#15326=AXIS2_PLACEMENT_3D('',#21170,#16969,#16970);
#15327=AXIS2_PLACEMENT_3D('',#21172,#16971,#16972);
#15328=AXIS2_PLACEMENT_3D('',#21185,#16974,#16975);
#15329=AXIS2_PLACEMENT_3D('',#21188,#16976,#16977);
#15330=AXIS2_PLACEMENT_3D('',#21205,#16978,#16979);
#15331=AXIS2_PLACEMENT_3D('',#21209,#16981,#16982);
#15332=AXIS2_PLACEMENT_3D('',#21211,#16984,#16985);
#15333=AXIS2_PLACEMENT_3D('',#21224,#16987,#16988);
#15334=AXIS2_PLACEMENT_3D('',#21245,#16990,#16991);
#15335=AXIS2_PLACEMENT_3D('',#21254,#16992,#16993);
#15336=AXIS2_PLACEMENT_3D('',#21265,#16994,#16995);
#15337=AXIS2_PLACEMENT_3D('',#21274,#16996,#16997);
#15338=AXIS2_PLACEMENT_3D('',#21285,#16998,#16999);
#15339=AXIS2_PLACEMENT_3D('',#21294,#17000,#17001);
#15340=AXIS2_PLACEMENT_3D('',#21298,#17003,#17004);
#15341=AXIS2_PLACEMENT_3D('',#21300,#17006,#17007);
#15342=AXIS2_PLACEMENT_3D('',#21310,#17013,#17014);
#15343=AXIS2_PLACEMENT_3D('',#21326,#17016,#17017);
#15344=AXIS2_PLACEMENT_3D('',#21328,#17019,#17020);
#15345=AXIS2_PLACEMENT_3D('',#21365,#17029,#17030);
#15346=AXIS2_PLACEMENT_3D('',#21367,#17031,#17032);
#15347=AXIS2_PLACEMENT_3D('',#21380,#17034,#17035);
#15348=AXIS2_PLACEMENT_3D('',#21383,#17036,#17037);
#15349=AXIS2_PLACEMENT_3D('',#21396,#17038,#17039);
#15350=AXIS2_PLACEMENT_3D('',#21398,#17040,#17041);
#15351=AXIS2_PLACEMENT_3D('',#21400,#17043,#17044);
#15352=AXIS2_PLACEMENT_3D('',#21413,#17046,#17047);
#15353=AXIS2_PLACEMENT_3D('',#21434,#17049,#17050);
#15354=AXIS2_PLACEMENT_3D('',#21443,#17051,#17052);
#15355=AXIS2_PLACEMENT_3D('',#21454,#17053,#17054);
#15356=AXIS2_PLACEMENT_3D('',#21463,#17055,#17056);
#15357=AXIS2_PLACEMENT_3D('',#21465,#17057,#17058);
#15358=AXIS2_PLACEMENT_3D('',#21467,#17060,#17061);
#15359=AXIS2_PLACEMENT_3D('',#21470,#17062,#17063);
#15360=AXIS2_PLACEMENT_3D('',#21474,#17065,#17066);
#15361=AXIS2_PLACEMENT_3D('',#21478,#17068,#17069);
#15362=AXIS2_PLACEMENT_3D('',#21482,#17071,#17072);
#15363=AXIS2_PLACEMENT_3D('',#21485,#17074,#17075);
#15364=AXIS2_PLACEMENT_3D('',#21487,#17076,#17077);
#15365=AXIS2_PLACEMENT_3D('',#21488,#17078,#17079);
#15366=AXIS2_PLACEMENT_3D('',#21490,#17081,#17082);
#15367=AXIS2_PLACEMENT_3D('',#21519,#17083,#17084);
#15368=AXIS2_PLACEMENT_3D('',#21521,#17085,#17086);
#15369=AXIS2_PLACEMENT_3D('',#21523,#17088,#17089);
#15370=AXIS2_PLACEMENT_3D('',#21525,#17090,#17091);
#15371=AXIS2_PLACEMENT_3D('',#21526,#17092,#17093);
#15372=AXIS2_PLACEMENT_3D('',#21527,#17094,#17095);
#15373=AXIS2_PLACEMENT_3D('',#21543,#17097,#17098);
#15374=AXIS2_PLACEMENT_3D('',#21558,#17099,#17100);
#15375=AXIS2_PLACEMENT_3D('',#21560,#17101,#17102);
#15376=AXIS2_PLACEMENT_3D('',#21562,#17103,#17104);
#15377=AXIS2_PLACEMENT_3D('',#21563,#17105,#17106);
#15378=AXIS2_PLACEMENT_3D('',#21564,#17107,#17108);
#15379=AXIS2_PLACEMENT_3D('',#21566,#17110,#17111);
#15380=AXIS2_PLACEMENT_3D('',#21568,#17113,#17114);
#15381=AXIS2_PLACEMENT_3D('',#21572,#17116,#17117);
#15382=AXIS2_PLACEMENT_3D('',#21574,#17119,#17120);
#15383=AXIS2_PLACEMENT_3D('',#21576,#17122,#17123);
#15384=AXIS2_PLACEMENT_3D('',#21577,#17124,#17125);
#15385=AXIS2_PLACEMENT_3D('',#21578,#17126,#17127);
#15386=AXIS2_PLACEMENT_3D('',#21580,#17128,#17129);
#15387=AXIS2_PLACEMENT_3D('',#21582,#17131,#17132);
#15388=AXIS2_PLACEMENT_3D('',#21584,#17133,#17134);
#15389=AXIS2_PLACEMENT_3D('',#21585,#17135,#17136);
#15390=AXIS2_PLACEMENT_3D('',#21586,#17137,#17138);
#15391=AXIS2_PLACEMENT_3D('',#21588,#17140,#17141);
#15392=AXIS2_PLACEMENT_3D('',#21590,#17143,#17144);
#15393=AXIS2_PLACEMENT_3D('',#21592,#17146,#17147);
#15394=AXIS2_PLACEMENT_3D('',#21593,#17148,#17149);
#15395=AXIS2_PLACEMENT_3D('',#21594,#17150,#17151);
#15396=AXIS2_PLACEMENT_3D('',#21595,#17152,#17153);
#15397=AXIS2_PLACEMENT_3D('',#21596,#17154,#17155);
#15398=AXIS2_PLACEMENT_3D('',#21598,#17157,#17158);
#15399=AXIS2_PLACEMENT_3D('',#21599,#17159,#17160);
#15400=AXIS2_PLACEMENT_3D('',#21600,#17161,#17162);
#15401=AXIS2_PLACEMENT_3D('',#21601,#17163,#17164);
#15402=AXIS2_PLACEMENT_3D('',#21602,#17165,#17166);
#15403=AXIS2_PLACEMENT_3D('',#21604,#17167,#17168);
#15404=AXIS2_PLACEMENT_3D('',#21606,#17169,#17170);
#15405=AXIS2_PLACEMENT_3D('',#21607,#17171,#17172);
#15406=AXIS2_PLACEMENT_3D('',#21608,#17173,#17174);
#15407=AXIS2_PLACEMENT_3D('',#21610,#17176,#17177);
#15408=AXIS2_PLACEMENT_3D('',#21613,#17179,#17180);
#15409=AXIS2_PLACEMENT_3D('',#21614,#17181,#17182);
#15410=AXIS2_PLACEMENT_3D('',#21616,#17183,#17184);
#15411=AXIS2_PLACEMENT_3D('',#21617,#17185,#17186);
#15412=AXIS2_PLACEMENT_3D('',#21618,#17187,#17188);
#15413=AXIS2_PLACEMENT_3D('',#21619,#17189,#17190);
#15414=AXIS2_PLACEMENT_3D('',#21621,#17192,#17193);
#15415=AXIS2_PLACEMENT_3D('',#21622,#17194,#17195);
#15416=AXIS2_PLACEMENT_3D('',#21624,#17196,#17197);
#15417=AXIS2_PLACEMENT_3D('',#21626,#17198,#17199);
#15418=AXIS2_PLACEMENT_3D('',#21627,#17200,#17201);
#15419=AXIS2_PLACEMENT_3D('',#21628,#17202,#17203);
#15420=AXIS2_PLACEMENT_3D('',#21629,#17204,#17205);
#15421=AXIS2_PLACEMENT_3D('',#21631,#17207,#17208);
#15422=AXIS2_PLACEMENT_3D('',#21633,#17210,#17211);
#15423=AXIS2_PLACEMENT_3D('',#21634,#17212,#17213);
#15424=AXIS2_PLACEMENT_3D('',#21637,#17215,#17216);
#15425=AXIS2_PLACEMENT_3D('',#21638,#17217,#17218);
#15426=AXIS2_PLACEMENT_3D('',#21640,#17219,#17220);
#15427=AXIS2_PLACEMENT_3D('',#21641,#17221,#17222);
#15428=AXIS2_PLACEMENT_3D('',#21642,#17223,#17224);
#15429=AXIS2_PLACEMENT_3D('',#21643,#17225,#17226);
#15430=AXIS2_PLACEMENT_3D('',#21645,#17228,#17229);
#15431=AXIS2_PLACEMENT_3D('',#21646,#17230,#17231);
#15432=AXIS2_PLACEMENT_3D('',#21649,#17233,#17234);
#15433=AXIS2_PLACEMENT_3D('',#21650,#17235,#17236);
#15434=AXIS2_PLACEMENT_3D('',#21652,#17237,#17238);
#15435=AXIS2_PLACEMENT_3D('',#21653,#17239,#17240);
#15436=AXIS2_PLACEMENT_3D('',#21654,#17241,#17242);
#15437=AXIS2_PLACEMENT_3D('',#21655,#17243,#17244);
#15438=AXIS2_PLACEMENT_3D('',#21657,#17246,#17247);
#15439=AXIS2_PLACEMENT_3D('',#21658,#17248,#17249);
#15440=AXIS2_PLACEMENT_3D('',#21659,#17250,#17251);
#15441=AXIS2_PLACEMENT_3D('',#21660,#17252,#17253);
#15442=AXIS2_PLACEMENT_3D('',#21661,#17254,#17255);
#15443=AXIS2_PLACEMENT_3D('',#21662,#17256,#17257);
#15444=AXIS2_PLACEMENT_3D('',#21663,#17258,#17259);
#15445=AXIS2_PLACEMENT_3D('',#21664,#17260,#17261);
#15446=AXIS2_PLACEMENT_3D('',#21665,#17262,#17263);
#15447=AXIS2_PLACEMENT_3D('',#21666,#17264,#17265);
#15448=AXIS2_PLACEMENT_3D('',#21667,#17266,#17267);
#15449=AXIS2_PLACEMENT_3D('',#21668,#17268,#17269);
#15450=AXIS2_PLACEMENT_3D('',#21669,#17270,#17271);
#15451=AXIS2_PLACEMENT_3D('',#21670,#17272,#17273);
#15452=AXIS2_PLACEMENT_3D('',#21671,#17274,#17275);
#15453=AXIS2_PLACEMENT_3D('',#21672,#17276,#17277);
#15454=AXIS2_PLACEMENT_3D('',#21673,#17278,#17279);
#15455=AXIS2_PLACEMENT_3D('',#21674,#17280,#17281);
#15456=AXIS2_PLACEMENT_3D('',#21675,#17282,#17283);
#15457=AXIS2_PLACEMENT_3D('',#21676,#17284,#17285);
#15458=AXIS2_PLACEMENT_3D('',#21677,#17286,#17287);
#15459=AXIS2_PLACEMENT_3D('',#21678,#17288,#17289);
#15460=AXIS2_PLACEMENT_3D('',#21679,#17290,#17291);
#15461=AXIS2_PLACEMENT_3D('',#21680,#17292,#17293);
#15462=AXIS2_PLACEMENT_3D('',#21682,#17294,#17295);
#15463=AXIS2_PLACEMENT_3D('',#21684,#17296,#17297);
#15464=AXIS2_PLACEMENT_3D('',#21685,#17298,#17299);
#15465=AXIS2_PLACEMENT_3D('',#21686,#17300,#17301);
#15466=AXIS2_PLACEMENT_3D('',#21688,#17302,#17303);
#15467=AXIS2_PLACEMENT_3D('',#22095,#17305,#17306);
#15468=AXIS2_PLACEMENT_3D('',#22178,#17307,#17308);
#15469=AXIS2_PLACEMENT_3D('',#22399,#17309,#17310);
#15470=AXIS2_PLACEMENT_3D('',#22483,#17311,#17312);
#15471=AXIS2_PLACEMENT_3D('',#22484,#17313,#17314);
#15472=AXIS2_PLACEMENT_3D('',#22594,#17315,#17316);
#15473=AXIS2_PLACEMENT_3D('',#22596,#17318,#17319);
#15474=AXIS2_PLACEMENT_3D('',#22597,#17320,#17321);
#15475=AXIS2_PLACEMENT_3D('',#22598,#17322,#17323);
#15476=AXIS2_PLACEMENT_3D('',#22599,#17324,#17325);
#15477=AXIS2_PLACEMENT_3D('',#22600,#17326,#17327);
#15478=AXIS2_PLACEMENT_3D('',#22602,#17328,#17329);
#15479=AXIS2_PLACEMENT_3D('',#22605,#17331,#17332);
#15480=AXIS2_PLACEMENT_3D('',#22606,#17333,#17334);
#15481=AXIS2_PLACEMENT_3D('',#22608,#17335,#17336);
#15482=AXIS2_PLACEMENT_3D('',#22609,#17337,#17338);
#15483=AXIS2_PLACEMENT_3D('',#22612,#17340,#17341);
#15484=AXIS2_PLACEMENT_3D('',#22613,#17342,#17343);
#15485=AXIS2_PLACEMENT_3D('',#22615,#17344,#17345);
#15486=AXIS2_PLACEMENT_3D('',#22616,#17346,#17347);
#15487=AXIS2_PLACEMENT_3D('',#22619,#17349,#17350);
#15488=AXIS2_PLACEMENT_3D('',#22620,#17351,#17352);
#15489=AXIS2_PLACEMENT_3D('',#22621,#17353,#17354);
#15490=AXIS2_PLACEMENT_3D('',#22622,#17355,#17356);
#15491=AXIS2_PLACEMENT_3D('',#22623,#17357,#17358);
#15492=AXIS2_PLACEMENT_3D('',#22624,#17359,#17360);
#15493=AXIS2_PLACEMENT_3D('',#22625,#17361,#17362);
#15494=AXIS2_PLACEMENT_3D('',#22626,#17363,#17364);
#15495=AXIS2_PLACEMENT_3D('',#22627,#17365,#17366);
#15496=AXIS2_PLACEMENT_3D('',#22629,#17367,#17368);
#15497=AXIS2_PLACEMENT_3D('',#22633,#17370,#17371);
#15498=AXIS2_PLACEMENT_3D('',#22634,#17372,#17373);
#15499=AXIS2_PLACEMENT_3D('',#22635,#17374,#17375);
#15500=AXIS2_PLACEMENT_3D('',#22637,#17376,#17377);
#15501=AXIS2_PLACEMENT_3D('',#22638,#17378,#17379);
#15502=AXIS2_PLACEMENT_3D('',#22641,#17381,#17382);
#15503=AXIS2_PLACEMENT_3D('',#22642,#17383,#17384);
#15504=AXIS2_PLACEMENT_3D('',#22644,#17385,#17386);
#15505=AXIS2_PLACEMENT_3D('',#22647,#17388,#17389);
#15506=AXIS2_PLACEMENT_3D('',#22648,#17390,#17391);
#15507=AXIS2_PLACEMENT_3D('',#22651,#17392,#17393);
#15508=AXIS2_PLACEMENT_3D('',#22655,#17395,#17396);
#15509=AXIS2_PLACEMENT_3D('',#22659,#17398,#17399);
#15510=AXIS2_PLACEMENT_3D('',#22663,#17401,#17402);
#15511=AXIS2_PLACEMENT_3D('',#22665,#17404,#17405);
#15512=AXIS2_PLACEMENT_3D('',#22703,#17407,#17408);
#15513=AXIS2_PLACEMENT_3D('',#22737,#17409,#17410);
#15514=AXIS2_PLACEMENT_3D('',#22741,#17412,#17413);
#15515=AXIS2_PLACEMENT_3D('',#22743,#17414,#17415);
#15516=AXIS2_PLACEMENT_3D('',#22847,#17419,#17420);
#15517=AXIS2_PLACEMENT_3D('',#22852,#17422,#17423);
#15518=AXIS2_PLACEMENT_3D('',#22855,#17425,#17426);
#15519=AXIS2_PLACEMENT_3D('',#22982,#17429,#17430);
#15520=AXIS2_PLACEMENT_3D('',#22986,#17433,#17434);
#15521=AXIS2_PLACEMENT_3D('',#23007,#17436,#17437);
#15522=AXIS2_PLACEMENT_3D('',#23010,#17439,#17440);
#15523=AXIS2_PLACEMENT_3D('',#23011,#17441,#17442);
#15524=AXIS2_PLACEMENT_3D('',#23014,#17444,#17445);
#15525=AXIS2_PLACEMENT_3D('',#23015,#17446,#17447);
#15526=AXIS2_PLACEMENT_3D('',#23019,#17449,#17450);
#15527=AXIS2_PLACEMENT_3D('',#23128,#17454,#17455);
#15528=AXIS2_PLACEMENT_3D('',#23133,#17457,#17458);
#15529=AXIS2_PLACEMENT_3D('',#23136,#17460,#17461);
#15530=AXIS2_PLACEMENT_3D('',#23263,#17464,#17465);
#15531=AXIS2_PLACEMENT_3D('',#23267,#17468,#17469);
#15532=AXIS2_PLACEMENT_3D('',#23269,#17470,#17471);
#15533=AXIS2_PLACEMENT_3D('',#23272,#17473,#17474);
#15534=AXIS2_PLACEMENT_3D('',#23273,#17475,#17476);
#15535=AXIS2_PLACEMENT_3D('',#23276,#17478,#17479);
#15536=AXIS2_PLACEMENT_3D('',#23277,#17480,#17481);
#15537=AXIS2_PLACEMENT_3D('',#23281,#17483,#17484);
#15538=AXIS2_PLACEMENT_3D('',#23284,#17486,#17487);
#15539=AXIS2_PLACEMENT_3D('',#23375,#17490,#17491);
#15540=AXIS2_PLACEMENT_3D('',#23379,#17493,#17494);
#15541=AXIS2_PLACEMENT_3D('',#23381,#17495,#17496);
#15542=AXIS2_PLACEMENT_3D('',#23481,#17500,#17501);
#15543=AXIS2_PLACEMENT_3D('',#23484,#17503,#17504);
#15544=AXIS2_PLACEMENT_3D('',#23485,#17505,#17506);
#15545=AXIS2_PLACEMENT_3D('',#23489,#17508,#17509);
#15546=AXIS2_PLACEMENT_3D('',#23557,#17513,#17514);
#15547=AXIS2_PLACEMENT_3D('',#23562,#17516,#17517);
#15548=AXIS2_PLACEMENT_3D('',#23565,#17519,#17520);
#15549=AXIS2_PLACEMENT_3D('',#23727,#17523,#17524);
#15550=AXIS2_PLACEMENT_3D('',#23731,#17527,#17528);
#15551=AXIS2_PLACEMENT_3D('',#23733,#17529,#17530);
#15552=AXIS2_PLACEMENT_3D('',#23736,#17532,#17533);
#15553=AXIS2_PLACEMENT_3D('',#23737,#17534,#17535);
#15554=AXIS2_PLACEMENT_3D('',#23740,#17537,#17538);
#15555=AXIS2_PLACEMENT_3D('',#23878,#17540,#17541);
#15556=AXIS2_PLACEMENT_3D('',#23894,#17542,#17543);
#15557=AXIS2_PLACEMENT_3D('',#23897,#17545,#17546);
#15558=AXIS2_PLACEMENT_3D('',#23947,#17547,#17548);
#15559=AXIS2_PLACEMENT_3D('',#23979,#17550,#17551);
#15560=AXIS2_PLACEMENT_3D('',#24137,#17554,#17555);
#15561=AXIS2_PLACEMENT_3D('',#24142,#17557,#17558);
#15562=AXIS2_PLACEMENT_3D('',#24156,#17559,#17560);
#15563=AXIS2_PLACEMENT_3D('',#24206,#17561,#17562);
#15564=AXIS2_PLACEMENT_3D('',#24208,#17563,#17564);
#15565=AXIS2_PLACEMENT_3D('',#24210,#17565,#17566);
#15566=AXIS2_PLACEMENT_3D('',#24211,#17567,#17568);
#15567=AXIS2_PLACEMENT_3D('',#24212,#17569,#17570);
#15568=AXIS2_PLACEMENT_3D('',#24214,#17571,#17572);
#15569=AXIS2_PLACEMENT_3D('',#24216,#17573,#17574);
#15570=AXIS2_PLACEMENT_3D('',#24220,#17576,#17577);
#15571=AXIS2_PLACEMENT_3D('',#24222,#17578,#17579);
#15572=AXIS2_PLACEMENT_3D('',#24224,#17580,#17581);
#15573=AXIS2_PLACEMENT_3D('',#24232,#17585,#17586);
#15574=AXIS2_PLACEMENT_3D('',#24234,#17587,#17588);
#15575=AXIS2_PLACEMENT_3D('',#24236,#17589,#17590);
#15576=AXIS2_PLACEMENT_3D('',#24239,#17592,#17593);
#15577=AXIS2_PLACEMENT_3D('',#24242,#17596,#17597);
#15578=AXIS2_PLACEMENT_3D('',#24244,#17598,#17599);
#15579=AXIS2_PLACEMENT_3D('',#24247,#17601,#17602);
#15580=AXIS2_PLACEMENT_3D('',#24248,#17603,#17604);
#15581=AXIS2_PLACEMENT_3D('',#24258,#17609,#17610);
#15582=AXIS2_PLACEMENT_3D('',#24260,#17611,#17612);
#15583=AXIS2_PLACEMENT_3D('',#24262,#17613,#17614);
#15584=AXIS2_PLACEMENT_3D('',#24264,#17615,#17616);
#15585=AXIS2_PLACEMENT_3D('',#24265,#17617,#17618);
#15586=AXIS2_PLACEMENT_3D('',#24268,#17620,#17621);
#15587=AXIS2_PLACEMENT_3D('',#24269,#17622,#17623);
#15588=AXIS2_PLACEMENT_3D('',#24272,#17625,#17626);
#15589=AXIS2_PLACEMENT_3D('',#24273,#17627,#17628);
#15590=AXIS2_PLACEMENT_3D('',#24276,#17630,#17631);
#15591=AXIS2_PLACEMENT_3D('',#24277,#17632,#17633);
#15592=AXIS2_PLACEMENT_3D('',#24280,#17635,#17636);
#15593=AXIS2_PLACEMENT_3D('',#24281,#17637,#17638);
#15594=AXIS2_PLACEMENT_3D('',#24284,#17640,#17641);
#15595=AXIS2_PLACEMENT_3D('',#24285,#17642,#17643);
#15596=AXIS2_PLACEMENT_3D('',#24288,#17645,#17646);
#15597=AXIS2_PLACEMENT_3D('',#24289,#17647,#17648);
#15598=AXIS2_PLACEMENT_3D('',#24292,#17650,#17651);
#15599=AXIS2_PLACEMENT_3D('',#24293,#17652,#17653);
#15600=AXIS2_PLACEMENT_3D('',#24296,#17655,#17656);
#15601=AXIS2_PLACEMENT_3D('',#24297,#17657,#17658);
#15602=AXIS2_PLACEMENT_3D('',#24315,#17660,#17661);
#15603=AXIS2_PLACEMENT_3D('',#24444,#17662,#17663);
#15604=AXIS2_PLACEMENT_3D('',#24467,#17664,#17665);
#15605=AXIS2_PLACEMENT_3D('',#24469,#17666,#17667);
#15606=AXIS2_PLACEMENT_3D('',#24471,#17669,#17670);
#15607=AXIS2_PLACEMENT_3D('',#24474,#17671,#17672);
#15608=AXIS2_PLACEMENT_3D('',#24493,#17675,#17676);
#15609=AXIS2_PLACEMENT_3D('',#24495,#17677,#17678);
#15610=AXIS2_PLACEMENT_3D('',#24497,#17679,#17680);
#15611=AXIS2_PLACEMENT_3D('',#24498,#17681,#17682);
#15612=AXIS2_PLACEMENT_3D('',#24499,#17683,#17684);
#15613=AXIS2_PLACEMENT_3D('',#24500,#17685,#17686);
#15614=AXIS2_PLACEMENT_3D('',#24502,#17688,#17689);
#15615=AXIS2_PLACEMENT_3D('',#24521,#17692,#17693);
#15616=AXIS2_PLACEMENT_3D('',#24523,#17694,#17695);
#15617=AXIS2_PLACEMENT_3D('',#24525,#17697,#17698);
#15618=AXIS2_PLACEMENT_3D('',#24526,#17699,#17700);
#15619=AXIS2_PLACEMENT_3D('',#24527,#17701,#17702);
#15620=AXIS2_PLACEMENT_3D('',#24528,#17703,#17704);
#15621=AXIS2_PLACEMENT_3D('',#24545,#17706,#17707);
#15622=AXIS2_PLACEMENT_3D('',#24546,#17708,#17709);
#15623=AXIS2_PLACEMENT_3D('',#24547,#17710,#17711);
#15624=AXIS2_PLACEMENT_3D('',#24553,#17715,#17716);
#15625=AXIS2_PLACEMENT_3D('',#24554,#17717,#17718);
#15626=AXIS2_PLACEMENT_3D('',#24555,#17719,#17720);
#15627=AXIS2_PLACEMENT_3D('',#24556,#17721,#17722);
#15628=AXIS2_PLACEMENT_3D('',#24557,#17723,#17724);
#15629=AXIS2_PLACEMENT_3D('',#24558,#17725,#17726);
#15630=AXIS2_PLACEMENT_3D('',#24559,#17727,#17728);
#15631=AXIS2_PLACEMENT_3D('',#24561,#17729,#17730);
#15632=AXIS2_PLACEMENT_3D('',#24562,#17731,#17732);
#15633=AXIS2_PLACEMENT_3D('',#24563,#17733,#17734);
#15634=AXIS2_PLACEMENT_3D('',#24582,#17737,#17738);
#15635=AXIS2_PLACEMENT_3D('',#24585,#17740,#17741);
#15636=AXIS2_PLACEMENT_3D('',#24587,#17743,#17744);
#15637=AXIS2_PLACEMENT_3D('',#24588,#17745,#17746);
#15638=AXIS2_PLACEMENT_3D('',#24589,#17747,#17748);
#15639=AXIS2_PLACEMENT_3D('',#24590,#17749,#17750);
#15640=AXIS2_PLACEMENT_3D('',#24591,#17751,#17752);
#15641=AXIS2_PLACEMENT_3D('',#24610,#17755,#17756);
#15642=AXIS2_PLACEMENT_3D('',#24612,#17758,#17759);
#15643=AXIS2_PLACEMENT_3D('',#24614,#17761,#17762);
#15644=AXIS2_PLACEMENT_3D('',#24615,#17763,#17764);
#15645=AXIS2_PLACEMENT_3D('',#24617,#17765,#17766);
#15646=AXIS2_PLACEMENT_3D('',#24620,#17768,#17769);
#15647=AXIS2_PLACEMENT_3D('',#24622,#17770,#17771);
#15648=AXIS2_PLACEMENT_3D('',#24625,#17773,#17774);
#15649=AXIS2_PLACEMENT_3D('',#24627,#17775,#17776);
#15650=AXIS2_PLACEMENT_3D('',#24629,#17777,#17778);
#15651=AXIS2_PLACEMENT_3D('',#24631,#17779,#17780);
#15652=AXIS2_PLACEMENT_3D('',#24633,#17781,#17782);
#15653=AXIS2_PLACEMENT_3D('',#24635,#17783,#17784);
#15654=AXIS2_PLACEMENT_3D('',#24636,#17785,#17786);
#15655=AXIS2_PLACEMENT_3D('',#24638,#17787,#17788);
#15656=AXIS2_PLACEMENT_3D('',#24640,#17789,#17790);
#15657=AXIS2_PLACEMENT_3D('',#24641,#17791,#17792);
#15658=AXIS2_PLACEMENT_3D('',#24642,#17793,#17794);
#15659=AXIS2_PLACEMENT_3D('',#24645,#17796,#17797);
#15660=AXIS2_PLACEMENT_3D('',#24646,#17798,#17799);
#15661=AXIS2_PLACEMENT_3D('',#24648,#17800,#17801);
#15662=AXIS2_PLACEMENT_3D('',#24649,#17802,#17803);
#15663=AXIS2_PLACEMENT_3D('',#24650,#17804,#17805);
#15664=AXIS2_PLACEMENT_3D('',#24652,#17806,#17807);
#15665=AXIS2_PLACEMENT_3D('',#24654,#17809,#17810);
#15666=AXIS2_PLACEMENT_3D('',#24655,#17811,#17812);
#15667=AXIS2_PLACEMENT_3D('',#24765,#17813,#17814);
#15668=AXIS2_PLACEMENT_3D('',#25020,#17815,#17816);
#15669=AXIS2_PLACEMENT_3D('',#25077,#17817,#17818);
#15670=AXIS2_PLACEMENT_3D('',#25079,#17819,#17820);
#15671=AXIS2_PLACEMENT_3D('',#25080,#17821,#17822);
#15672=AXIS2_PLACEMENT_3D('',#25082,#17823,#17824);
#15673=AXIS2_PLACEMENT_3D('',#25098,#17825,#17826);
#15674=AXIS2_PLACEMENT_3D('',#25099,#17827,#17828);
#15675=AXIS2_PLACEMENT_3D('',#25101,#17829,#17830);
#15676=AXIS2_PLACEMENT_3D('',#25102,#17831,#17832);
#15677=AXIS2_PLACEMENT_3D('',#25104,#17833,#17834);
#15678=AXIS2_PLACEMENT_3D('',#25105,#17835,#17836);
#15679=AXIS2_PLACEMENT_3D('',#25129,#17837,#17838);
#15680=AXIS2_PLACEMENT_3D('',#25145,#17839,#17840);
#15681=AXIS2_PLACEMENT_3D('',#25146,#17841,#17842);
#15682=AXIS2_PLACEMENT_3D('',#25150,#17844,#17845);
#15683=AXIS2_PLACEMENT_3D('',#25153,#17847,#17848);
#15684=AXIS2_PLACEMENT_3D('',#25155,#17850,#17851);
#15685=AXIS2_PLACEMENT_3D('',#25173,#17852,#17853);
#15686=AXIS2_PLACEMENT_3D('',#25189,#17854,#17855);
#15687=AXIS2_PLACEMENT_3D('',#25190,#17856,#17857);
#15688=AXIS2_PLACEMENT_3D('',#25192,#17858,#17859);
#15689=AXIS2_PLACEMENT_3D('',#25194,#17860,#17861);
#15690=AXIS2_PLACEMENT_3D('',#25195,#17862,#17863);
#15691=AXIS2_PLACEMENT_3D('',#25197,#17864,#17865);
#15692=AXIS2_PLACEMENT_3D('',#25198,#17866,#17867);
#15693=AXIS2_PLACEMENT_3D('',#25216,#17868,#17869);
#15694=AXIS2_PLACEMENT_3D('',#25232,#17870,#17871);
#15695=AXIS2_PLACEMENT_3D('',#25233,#17872,#17873);
#15696=AXIS2_PLACEMENT_3D('',#25235,#17874,#17875);
#15697=AXIS2_PLACEMENT_3D('',#25237,#17876,#17877);
#15698=AXIS2_PLACEMENT_3D('',#25238,#17878,#17879);
#15699=AXIS2_PLACEMENT_3D('',#25240,#17880,#17881);
#15700=AXIS2_PLACEMENT_3D('',#25241,#17882,#17883);
#15701=AXIS2_PLACEMENT_3D('',#25243,#17884,#17885);
#15702=AXIS2_PLACEMENT_3D('',#25244,#17886,#17887);
#15703=AXIS2_PLACEMENT_3D('',#25246,#17889,#17890);
#15704=AXIS2_PLACEMENT_3D('',#25247,#17891,#17892);
#15705=AXIS2_PLACEMENT_3D('',#25248,#17893,#17894);
#15706=AXIS2_PLACEMENT_3D('',#25249,#17895,#17896);
#15707=AXIS2_PLACEMENT_3D('',#25252,#17898,#17899);
#15708=AXIS2_PLACEMENT_3D('',#25257,#17902,#17903);
#15709=AXIS2_PLACEMENT_3D('',#25259,#17905,#17906);
#15710=AXIS2_PLACEMENT_3D('',#25261,#17908,#17909);
#15711=AXIS2_PLACEMENT_3D('',#25263,#17910,#17911);
#15712=AXIS2_PLACEMENT_3D('',#25265,#17912,#17913);
#15713=AXIS2_PLACEMENT_3D('',#25266,#17914,#17915);
#15714=AXIS2_PLACEMENT_3D('',#25267,#17916,#17917);
#15715=AXIS2_PLACEMENT_3D('',#25269,#17918,#17919);
#15716=AXIS2_PLACEMENT_3D('',#25271,#17921,#17922);
#15717=AXIS2_PLACEMENT_3D('',#25273,#17923,#17924);
#15718=AXIS2_PLACEMENT_3D('',#25274,#17925,#17926);
#15719=AXIS2_PLACEMENT_3D('',#25275,#17927,#17928);
#15720=AXIS2_PLACEMENT_3D('',#25277,#17929,#17930);
#15721=AXIS2_PLACEMENT_3D('',#25278,#17931,#17932);
#15722=AXIS2_PLACEMENT_3D('',#25279,#17933,#17934);
#15723=AXIS2_PLACEMENT_3D('',#25281,#17935,#17936);
#15724=AXIS2_PLACEMENT_3D('',#25282,#17937,#17938);
#15725=AXIS2_PLACEMENT_3D('',#25283,#17939,#17940);
#15726=AXIS2_PLACEMENT_3D('',#25285,#17941,#17942);
#15727=AXIS2_PLACEMENT_3D('',#25286,#17943,#17944);
#15728=AXIS2_PLACEMENT_3D('',#25287,#17945,#17946);
#15729=AXIS2_PLACEMENT_3D('',#25290,#17949,#17950);
#15730=AXIS2_PLACEMENT_3D('',#25292,#17951,#17952);
#15731=AXIS2_PLACEMENT_3D('',#25295,#17955,#17956);
#15732=AXIS2_PLACEMENT_3D('',#25297,#17958,#17959);
#15733=AXIS2_PLACEMENT_3D('',#25299,#17961,#17962);
#15734=AXIS2_PLACEMENT_3D('',#25312,#17964,#17965);
#15735=AXIS2_PLACEMENT_3D('',#25314,#17967,#17968);
#15736=AXIS2_PLACEMENT_3D('',#25315,#17969,#17970);
#15737=AXIS2_PLACEMENT_3D('',#25330,#17971,#17972);
#15738=AXIS2_PLACEMENT_3D('',#25331,#17973,#17974);
#15739=AXIS2_PLACEMENT_3D('',#25332,#17975,#17976);
#15740=AXIS2_PLACEMENT_3D('',#25333,#17977,#17978);
#15741=AXIS2_PLACEMENT_3D('',#25335,#17980,#17981);
#15742=AXIS2_PLACEMENT_3D('',#25338,#17983,#17984);
#15743=AXIS2_PLACEMENT_3D('',#25339,#17985,#17986);
#15744=AXIS2_PLACEMENT_3D('',#25342,#17988,#17989);
#15745=AXIS2_PLACEMENT_3D('',#25343,#17990,#17991);
#15746=AXIS2_PLACEMENT_3D('',#25345,#17992,#17993);
#15747=AXIS2_PLACEMENT_3D('',#25346,#17994,#17995);
#15748=AXIS2_PLACEMENT_3D('',#25347,#17996,#17997);
#15749=AXIS2_PLACEMENT_3D('',#25348,#17998,#17999);
#15750=AXIS2_PLACEMENT_3D('',#25350,#18000,#18001);
#15751=AXIS2_PLACEMENT_3D('',#25351,#18002,#18003);
#15752=AXIS2_PLACEMENT_3D('',#25352,#18004,#18005);
#15753=AXIS2_PLACEMENT_3D('',#25353,#18006,#18007);
#15754=AXIS2_PLACEMENT_3D('',#25354,#18008,#18009);
#15755=AXIS2_PLACEMENT_3D('',#25355,#18010,#18011);
#15756=AXIS2_PLACEMENT_3D('',#25356,#18012,#18013);
#15757=AXIS2_PLACEMENT_3D('',#25357,#18014,#18015);
#15758=AXIS2_PLACEMENT_3D('',#25358,#18016,#18017);
#15759=AXIS2_PLACEMENT_3D('',#25359,#18018,#18019);
#15760=AXIS2_PLACEMENT_3D('',#25360,#18020,#18021);
#15761=AXIS2_PLACEMENT_3D('',#25361,#18022,#18023);
#15762=AXIS2_PLACEMENT_3D('',#25362,#18024,#18025);
#15763=AXIS2_PLACEMENT_3D('',#25363,#18026,#18027);
#15764=AXIS2_PLACEMENT_3D('',#25364,#18028,#18029);
#15765=AXIS2_PLACEMENT_3D('',#25365,#18030,#18031);
#15766=AXIS2_PLACEMENT_3D('',#25367,#18033,#18034);
#15767=AXIS2_PLACEMENT_3D('',#25368,#18035,#18036);
#15768=AXIS2_PLACEMENT_3D('',#25370,#18038,#18039);
#15769=AXIS2_PLACEMENT_3D('',#25371,#18040,#18041);
#15770=AXIS2_PLACEMENT_3D('',#25372,#18042,#18043);
#15771=AXIS2_PLACEMENT_3D('',#25373,#18044,#18045);
#15772=AXIS2_PLACEMENT_3D('',#25374,#18046,#18047);
#15773=AXIS2_PLACEMENT_3D('',#25375,#18048,#18049);
#15774=AXIS2_PLACEMENT_3D('',#25377,#18051,#18052);
#15775=AXIS2_PLACEMENT_3D('',#25379,#18054,#18055);
#15776=AXIS2_PLACEMENT_3D('',#25381,#18056,#18057);
#15777=AXIS2_PLACEMENT_3D('',#25383,#18059,#18060);
#15778=AXIS2_PLACEMENT_3D('',#25385,#18062,#18063);
#15779=AXIS2_PLACEMENT_3D('',#25387,#18065,#18066);
#15780=AXIS2_PLACEMENT_3D('',#25388,#18067,#18068);
#15781=AXIS2_PLACEMENT_3D('',#25389,#18069,#18070);
#15782=AXIS2_PLACEMENT_3D('',#25390,#18071,#18072);
#15783=AXIS2_PLACEMENT_3D('',#25391,#18073,#18074);
#15784=AXIS2_PLACEMENT_3D('',#25392,#18075,#18076);
#15785=AXIS2_PLACEMENT_3D('',#25393,#18077,#18078);
#15786=AXIS2_PLACEMENT_3D('',#25394,#18079,#18080);
#15787=AXIS2_PLACEMENT_3D('',#25395,#18081,#18082);
#15788=AXIS2_PLACEMENT_3D('',#25396,#18083,#18084);
#15789=AXIS2_PLACEMENT_3D('',#25397,#18085,#18086);
#15790=AXIS2_PLACEMENT_3D('',#25398,#18087,#18088);
#15791=AXIS2_PLACEMENT_3D('',#25399,#18089,#18090);
#15792=AXIS2_PLACEMENT_3D('',#25400,#18091,#18092);
#15793=AXIS2_PLACEMENT_3D('',#25403,#18094,#18095);
#15794=AXIS2_PLACEMENT_3D('',#25404,#18096,#18097);
#15795=AXIS2_PLACEMENT_3D('',#25406,#18098,#18099);
#15796=AXIS2_PLACEMENT_3D('',#25407,#18100,#18101);
#15797=AXIS2_PLACEMENT_3D('',#25409,#18103,#18104);
#15798=AXIS2_PLACEMENT_3D('',#25410,#18105,#18106);
#15799=AXIS2_PLACEMENT_3D('',#25411,#18107,#18108);
#15800=AXIS2_PLACEMENT_3D('',#25412,#18109,#18110);
#15801=AXIS2_PLACEMENT_3D('',#25415,#18111,#18112);
#15802=AXIS2_PLACEMENT_3D('',#25419,#18114,#18115);
#15803=AXIS2_PLACEMENT_3D('',#25421,#18117,#18118);
#15804=AXIS2_PLACEMENT_3D('',#25427,#18122,#18123);
#15805=AXIS2_PLACEMENT_3D('',#25429,#18124,#18125);
#15806=AXIS2_PLACEMENT_3D('',#25431,#18126,#18127);
#15807=AXIS2_PLACEMENT_3D('',#25435,#18129,#18130);
#15808=AXIS2_PLACEMENT_3D('',#25437,#18131,#18132);
#15809=AXIS2_PLACEMENT_3D('',#25438,#18133,#18134);
#15810=AXIS2_PLACEMENT_3D('',#25439,#18135,#18136);
#15811=AXIS2_PLACEMENT_3D('',#25441,#18137,#18138);
#15812=AXIS2_PLACEMENT_3D('',#25443,#18140,#18141);
#15813=AXIS2_PLACEMENT_3D('',#25446,#18143,#18144);
#15814=AXIS2_PLACEMENT_3D('',#25448,#18145,#18146);
#15815=AXIS2_PLACEMENT_3D('',#25449,#18147,#18148);
#15816=AXIS2_PLACEMENT_3D('',#25452,#18149,#18150);
#15817=AXIS2_PLACEMENT_3D('',#25455,#18153,#18154);
#15818=AXIS2_PLACEMENT_3D('',#25456,#18155,#18156);
#15819=AXIS2_PLACEMENT_3D('',#25458,#18157,#18158);
#15820=AXIS2_PLACEMENT_3D('',#25459,#18159,#18160);
#15821=AXIS2_PLACEMENT_3D('',#25462,#18162,#18163);
#15822=AXIS2_PLACEMENT_3D('',#25463,#18164,#18165);
#15823=AXIS2_PLACEMENT_3D('',#25465,#18167,#18168);
#15824=AXIS2_PLACEMENT_3D('',#25467,#18170,#18171);
#15825=AXIS2_PLACEMENT_3D('',#25468,#18172,#18173);
#15826=AXIS2_PLACEMENT_3D('',#25469,#18174,#18175);
#15827=AXIS2_PLACEMENT_3D('',#25472,#18176,#18177);
#15828=AXIS2_PLACEMENT_3D('',#25473,#18178,#18179);
#15829=AXIS2_PLACEMENT_3D('',#25476,#18181,#18182);
#15830=AXIS2_PLACEMENT_3D('',#25477,#18183,#18184);
#15831=AXIS2_PLACEMENT_3D('',#25479,#18185,#18186);
#15832=AXIS2_PLACEMENT_3D('',#25481,#18187,#18188);
#15833=AXIS2_PLACEMENT_3D('',#25483,#18189,#18190);
#15834=AXIS2_PLACEMENT_3D('',#25485,#18191,#18192);
#15835=AXIS2_PLACEMENT_3D('',#25487,#18193,#18194);
#15836=AXIS2_PLACEMENT_3D('',#25489,#18195,#18196);
#15837=AXIS2_PLACEMENT_3D('',#25491,#18197,#18198);
#15838=AXIS2_PLACEMENT_3D('',#25496,#18200,#18201);
#15839=AXIS2_PLACEMENT_3D('',#25500,#18204,#18205);
#15840=AXIS2_PLACEMENT_3D('',#25502,#18206,#18207);
#15841=AXIS2_PLACEMENT_3D('',#25504,#18209,#18210);
#15842=AXIS2_PLACEMENT_3D('',#25508,#18212,#18213);
#15843=AXIS2_PLACEMENT_3D('',#25510,#18215,#18216);
#15844=AXIS2_PLACEMENT_3D('',#25512,#18217,#18218);
#15845=AXIS2_PLACEMENT_3D('',#25516,#18221,#18222);
#15846=AXIS2_PLACEMENT_3D('',#25518,#18224,#18225);
#15847=AXIS2_PLACEMENT_3D('',#25524,#18229,#18230);
#15848=AXIS2_PLACEMENT_3D('',#25528,#18233,#18234);
#15849=AXIS2_PLACEMENT_3D('',#25530,#18235,#18236);
#15850=AXIS2_PLACEMENT_3D('',#25532,#18237,#18238);
#15851=AXIS2_PLACEMENT_3D('',#25534,#18239,#18240);
#15852=AXIS2_PLACEMENT_3D('',#25536,#18242,#18243);
#15853=AXIS2_PLACEMENT_3D('',#25538,#18245,#18246);
#15854=AXIS2_PLACEMENT_3D('',#25542,#18249,#18250);
#15855=AXIS2_PLACEMENT_3D('',#25546,#18253,#18254);
#15856=AXIS2_PLACEMENT_3D('',#25548,#18256,#18257);
#15857=AXIS2_PLACEMENT_3D('',#25550,#18258,#18259);
#15858=AXIS2_PLACEMENT_3D('',#25552,#18260,#18261);
#15859=AXIS2_PLACEMENT_3D('',#25554,#18262,#18263);
#15860=AXIS2_PLACEMENT_3D('',#25556,#18264,#18265);
#15861=AXIS2_PLACEMENT_3D('',#25558,#18266,#18267);
#15862=AXIS2_PLACEMENT_3D('',#25560,#18268,#18269);
#15863=AXIS2_PLACEMENT_3D('',#25562,#18270,#18271);
#15864=AXIS2_PLACEMENT_3D('',#25564,#18272,#18273);
#15865=AXIS2_PLACEMENT_3D('',#25565,#18274,#18275);
#15866=AXIS2_PLACEMENT_3D('',#25568,#18277,#18278);
#15867=AXIS2_PLACEMENT_3D('',#25569,#18279,#18280);
#15868=AXIS2_PLACEMENT_3D('',#25572,#18282,#18283);
#15869=AXIS2_PLACEMENT_3D('',#25573,#18284,#18285);
#15870=AXIS2_PLACEMENT_3D('',#25574,#18286,#18287);
#15871=AXIS2_PLACEMENT_3D('',#25577,#18289,#18290);
#15872=AXIS2_PLACEMENT_3D('',#25578,#18291,#18292);
#15873=AXIS2_PLACEMENT_3D('',#25581,#18294,#18295);
#15874=AXIS2_PLACEMENT_3D('',#25582,#18296,#18297);
#15875=AXIS2_PLACEMENT_3D('',#25583,#18298,#18299);
#15876=AXIS2_PLACEMENT_3D('',#25586,#18301,#18302);
#15877=AXIS2_PLACEMENT_3D('',#25587,#18303,#18304);
#15878=AXIS2_PLACEMENT_3D('',#25590,#18306,#18307);
#15879=AXIS2_PLACEMENT_3D('',#25591,#18308,#18309);
#15880=AXIS2_PLACEMENT_3D('',#25592,#18310,#18311);
#15881=AXIS2_PLACEMENT_3D('',#25595,#18313,#18314);
#15882=AXIS2_PLACEMENT_3D('',#25596,#18315,#18316);
#15883=AXIS2_PLACEMENT_3D('',#25599,#18318,#18319);
#15884=AXIS2_PLACEMENT_3D('',#25600,#18320,#18321);
#15885=AXIS2_PLACEMENT_3D('',#25601,#18322,#18323);
#15886=AXIS2_PLACEMENT_3D('',#25604,#18325,#18326);
#15887=AXIS2_PLACEMENT_3D('',#25605,#18327,#18328);
#15888=AXIS2_PLACEMENT_3D('',#25608,#18330,#18331);
#15889=AXIS2_PLACEMENT_3D('',#25609,#18332,#18333);
#15890=AXIS2_PLACEMENT_3D('',#25610,#18334,#18335);
#15891=AXIS2_PLACEMENT_3D('',#25613,#18337,#18338);
#15892=AXIS2_PLACEMENT_3D('',#25614,#18339,#18340);
#15893=AXIS2_PLACEMENT_3D('',#25617,#18342,#18343);
#15894=AXIS2_PLACEMENT_3D('',#25618,#18344,#18345);
#15895=AXIS2_PLACEMENT_3D('',#25619,#18346,#18347);
#15896=AXIS2_PLACEMENT_3D('',#25622,#18349,#18350);
#15897=AXIS2_PLACEMENT_3D('',#25623,#18351,#18352);
#15898=AXIS2_PLACEMENT_3D('',#25626,#18354,#18355);
#15899=AXIS2_PLACEMENT_3D('',#25627,#18356,#18357);
#15900=AXIS2_PLACEMENT_3D('',#25628,#18358,#18359);
#15901=AXIS2_PLACEMENT_3D('',#25630,#18361,#18362);
#15902=AXIS2_PLACEMENT_3D('',#25631,#18363,#18364);
#15903=AXIS2_PLACEMENT_3D('',#25634,#18365,#18366);
#15904=AXIS2_PLACEMENT_3D('',#25638,#18368,#18369);
#15905=AXIS2_PLACEMENT_3D('',#25640,#18371,#18372);
#15906=AXIS2_PLACEMENT_3D('',#25646,#18376,#18377);
#15907=AXIS2_PLACEMENT_3D('',#25648,#18378,#18379);
#15908=AXIS2_PLACEMENT_3D('',#25650,#18380,#18381);
#15909=AXIS2_PLACEMENT_3D('',#25652,#18383,#18384);
#15910=AXIS2_PLACEMENT_3D('',#25655,#18385,#18386);
#15911=AXIS2_PLACEMENT_3D('',#25659,#18388,#18389);
#15912=AXIS2_PLACEMENT_3D('',#25661,#18391,#18392);
#15913=AXIS2_PLACEMENT_3D('',#25667,#18396,#18397);
#15914=AXIS2_PLACEMENT_3D('',#25669,#18398,#18399);
#15915=AXIS2_PLACEMENT_3D('',#25671,#18400,#18401);
#15916=AXIS2_PLACEMENT_3D('',#25673,#18403,#18404);
#15917=AXIS2_PLACEMENT_3D('',#25676,#18405,#18406);
#15918=AXIS2_PLACEMENT_3D('',#25680,#18408,#18409);
#15919=AXIS2_PLACEMENT_3D('',#25682,#18411,#18412);
#15920=AXIS2_PLACEMENT_3D('',#25688,#18416,#18417);
#15921=AXIS2_PLACEMENT_3D('',#25690,#18418,#18419);
#15922=AXIS2_PLACEMENT_3D('',#25692,#18420,#18421);
#15923=AXIS2_PLACEMENT_3D('',#25694,#18423,#18424);
#15924=AXIS2_PLACEMENT_3D('',#25697,#18425,#18426);
#15925=AXIS2_PLACEMENT_3D('',#25701,#18428,#18429);
#15926=AXIS2_PLACEMENT_3D('',#25703,#18431,#18432);
#15927=AXIS2_PLACEMENT_3D('',#25709,#18436,#18437);
#15928=AXIS2_PLACEMENT_3D('',#25711,#18438,#18439);
#15929=AXIS2_PLACEMENT_3D('',#25713,#18440,#18441);
#15930=AXIS2_PLACEMENT_3D('',#25715,#18443,#18444);
#15931=AXIS2_PLACEMENT_3D('',#25716,#18445,#18446);
#15932=AXIS2_PLACEMENT_3D('',#25717,#18447,#18448);
#15933=AXIS2_PLACEMENT_3D('',#25718,#18449,#18450);
#15934=AXIS2_PLACEMENT_3D('',#25719,#18451,#18452);
#15935=AXIS2_PLACEMENT_3D('',#25720,#18453,#18454);
#15936=AXIS2_PLACEMENT_3D('',#25721,#18455,#18456);
#15937=AXIS2_PLACEMENT_3D('',#25722,#18457,#18458);
#15938=AXIS2_PLACEMENT_3D('',#25723,#18459,#18460);
#15939=AXIS2_PLACEMENT_3D('',#25724,#18461,#18462);
#15940=AXIS2_PLACEMENT_3D('',#25725,#18463,#18464);
#15941=AXIS2_PLACEMENT_3D('',#25726,#18465,#18466);
#15942=AXIS2_PLACEMENT_3D('',#25727,#18467,#18468);
#15943=AXIS2_PLACEMENT_3D('',#25729,#18469,#18470);
#15944=AXIS2_PLACEMENT_3D('',#25732,#18472,#18473);
#15945=AXIS2_PLACEMENT_3D('',#25733,#18474,#18475);
#15946=AXIS2_PLACEMENT_3D('',#25735,#18476,#18477);
#15947=AXIS2_PLACEMENT_3D('',#25736,#18478,#18479);
#15948=AXIS2_PLACEMENT_3D('',#25738,#18480,#18481);
#15949=AXIS2_PLACEMENT_3D('',#25740,#18483,#18484);
#15950=AXIS2_PLACEMENT_3D('',#25741,#18485,#18486);
#15951=AXIS2_PLACEMENT_3D('',#25742,#18487,#18488);
#15952=AXIS2_PLACEMENT_3D('',#25756,#18491,#18492);
#15953=AXIS2_PLACEMENT_3D('',#25770,#18495,#18496);
#15954=AXIS2_PLACEMENT_3D('',#25771,#18497,#18498);
#15955=AXIS2_PLACEMENT_3D('',#25777,#18499,#18500);
#15956=AXIS2_PLACEMENT_3D('',#25781,#18501,#18502);
#15957=AXIS2_PLACEMENT_3D('',#25793,#18507,#18508);
#15958=AXIS2_PLACEMENT_3D('',#25797,#18511,#18512);
#15959=AXIS2_PLACEMENT_3D('',#25807,#18516,#18517);
#15960=AXIS2_PLACEMENT_3D('',#25821,#18520,#18521);
#15961=AXIS2_PLACEMENT_3D('',#25835,#18524,#18525);
#15962=AXIS2_PLACEMENT_3D('',#25836,#18526,#18527);
#15963=AXIS2_PLACEMENT_3D('',#25842,#18528,#18529);
#15964=AXIS2_PLACEMENT_3D('',#25846,#18530,#18531);
#15965=AXIS2_PLACEMENT_3D('',#25858,#18536,#18537);
#15966=AXIS2_PLACEMENT_3D('',#25862,#18540,#18541);
#15967=AXIS2_PLACEMENT_3D('',#25872,#18545,#18546);
#15968=AXIS2_PLACEMENT_3D('',#25886,#18549,#18550);
#15969=AXIS2_PLACEMENT_3D('',#25900,#18553,#18554);
#15970=AXIS2_PLACEMENT_3D('',#25901,#18555,#18556);
#15971=AXIS2_PLACEMENT_3D('',#25907,#18557,#18558);
#15972=AXIS2_PLACEMENT_3D('',#25911,#18559,#18560);
#15973=AXIS2_PLACEMENT_3D('',#25923,#18565,#18566);
#15974=AXIS2_PLACEMENT_3D('',#25927,#18569,#18570);
#15975=AXIS2_PLACEMENT_3D('',#25937,#18574,#18575);
#15976=AXIS2_PLACEMENT_3D('',#25951,#18578,#18579);
#15977=AXIS2_PLACEMENT_3D('',#25965,#18582,#18583);
#15978=AXIS2_PLACEMENT_3D('',#25966,#18584,#18585);
#15979=AXIS2_PLACEMENT_3D('',#25972,#18586,#18587);
#15980=AXIS2_PLACEMENT_3D('',#25976,#18588,#18589);
#15981=AXIS2_PLACEMENT_3D('',#25988,#18594,#18595);
#15982=AXIS2_PLACEMENT_3D('',#25992,#18598,#18599);
#15983=AXIS2_PLACEMENT_3D('',#26002,#18603,#18604);
#15984=AXIS2_PLACEMENT_3D('',#26015,#18607,#18608);
#15985=AXIS2_PLACEMENT_3D('',#26031,#18613,#18614);
#15986=AXIS2_PLACEMENT_3D('',#26045,#18617,#18618);
#15987=AXIS2_PLACEMENT_3D('',#26047,#18619,#18620);
#15988=AXIS2_PLACEMENT_3D('',#26048,#18621,#18622);
#15989=AXIS2_PLACEMENT_3D('',#26052,#18623,#18624);
#15990=AXIS2_PLACEMENT_3D('',#26064,#18629,#18630);
#15991=AXIS2_PLACEMENT_3D('',#26066,#18631,#18632);
#15992=AXIS2_PLACEMENT_3D('',#26075,#18633,#18634);
#15993=AXIS2_PLACEMENT_3D('',#26076,#18635,#18636);
#15994=AXIS2_PLACEMENT_3D('',#26078,#18637,#18638);
#15995=AXIS2_PLACEMENT_3D('',#26082,#18640,#18641);
#15996=AXIS2_PLACEMENT_3D('',#26086,#18643,#18644);
#15997=AXIS2_PLACEMENT_3D('',#26090,#18646,#18647);
#15998=AXIS2_PLACEMENT_3D('',#26094,#18649,#18650);
#15999=AXIS2_PLACEMENT_3D('',#26098,#18652,#18653);
#16000=AXIS2_PLACEMENT_3D('',#26102,#18655,#18656);
#16001=AXIS2_PLACEMENT_3D('',#26106,#18658,#18659);
#16002=AXIS2_PLACEMENT_3D('',#26108,#18661,#18662);
#16003=AXIS2_PLACEMENT_3D('',#26109,#18663,#18664);
#16004=AXIS2_PLACEMENT_3D('',#26110,#18665,#18666);
#16005=AXIS2_PLACEMENT_3D('',#26111,#18667,#18668);
#16006=AXIS2_PLACEMENT_3D('',#26113,#18669,#18670);
#16007=AXIS2_PLACEMENT_3D('',#26117,#18672,#18673);
#16008=AXIS2_PLACEMENT_3D('',#26121,#18675,#18676);
#16009=AXIS2_PLACEMENT_3D('',#26125,#18678,#18679);
#16010=AXIS2_PLACEMENT_3D('',#26129,#18681,#18682);
#16011=AXIS2_PLACEMENT_3D('',#26133,#18684,#18685);
#16012=AXIS2_PLACEMENT_3D('',#26137,#18687,#18688);
#16013=AXIS2_PLACEMENT_3D('',#26141,#18690,#18691);
#16014=AXIS2_PLACEMENT_3D('',#26145,#18693,#18694);
#16015=AXIS2_PLACEMENT_3D('',#26148,#18696,#18697);
#16016=AXIS2_PLACEMENT_3D('',#26149,#18698,#18699);
#16017=AXIS2_PLACEMENT_3D('',#26156,#18701,#18702);
#16018=AXIS2_PLACEMENT_3D('',#26167,#18704,#18705);
#16019=AXIS2_PLACEMENT_3D('',#26173,#18706,#18707);
#16020=AXIS2_PLACEMENT_3D('',#26177,#18708,#18709);
#16021=AXIS2_PLACEMENT_3D('',#26185,#18714,#18715);
#16022=AXIS2_PLACEMENT_3D('',#26189,#18718,#18719);
#16023=AXIS2_PLACEMENT_3D('',#26199,#18723,#18724);
#16024=AXIS2_PLACEMENT_3D('',#26210,#18726,#18727);
#16025=AXIS2_PLACEMENT_3D('',#26221,#18729,#18730);
#16026=AXIS2_PLACEMENT_3D('',#26227,#18731,#18732);
#16027=AXIS2_PLACEMENT_3D('',#26231,#18733,#18734);
#16028=AXIS2_PLACEMENT_3D('',#26243,#18739,#18740);
#16029=AXIS2_PLACEMENT_3D('',#26247,#18743,#18744);
#16030=AXIS2_PLACEMENT_3D('',#26257,#18748,#18749);
#16031=AXIS2_PLACEMENT_3D('',#26266,#18754,#18755);
#16032=AXIS2_PLACEMENT_3D('',#26272,#18759,#18760);
#16033=AXIS2_PLACEMENT_3D('',#26281,#18765,#18766);
#16034=AXIS2_PLACEMENT_3D('',#26287,#18770,#18771);
#16035=AXIS2_PLACEMENT_3D('',#26296,#18776,#18777);
#16036=AXIS2_PLACEMENT_3D('',#26302,#18781,#18782);
#16037=AXIS2_PLACEMENT_3D('',#26311,#18787,#18788);
#16038=AXIS2_PLACEMENT_3D('',#26317,#18792,#18793);
#16039=AXIS2_PLACEMENT_3D('',#26326,#18798,#18799);
#16040=AXIS2_PLACEMENT_3D('',#26332,#18803,#18804);
#16041=AXIS2_PLACEMENT_3D('',#26335,#18807,#18808);
#16042=AXIS2_PLACEMENT_3D('',#26336,#18809,#18810);
#16043=AXIS2_PLACEMENT_3D('',#26339,#18813,#18814);
#16044=AXIS2_PLACEMENT_3D('',#26340,#18815,#18816);
#16045=AXIS2_PLACEMENT_3D('',#26343,#18819,#18820);
#16046=AXIS2_PLACEMENT_3D('',#26345,#18822,#18823);
#16047=AXIS2_PLACEMENT_3D('',#26348,#18826,#18827);
#16048=AXIS2_PLACEMENT_3D('',#26349,#18828,#18829);
#16049=AXIS2_PLACEMENT_3D('',#26352,#18832,#18833);
#16050=AXIS2_PLACEMENT_3D('',#26353,#18834,#18835);
#16051=AXIS2_PLACEMENT_3D('',#26356,#18838,#18839);
#16052=AXIS2_PLACEMENT_3D('',#26357,#18840,#18841);
#16053=AXIS2_PLACEMENT_3D('',#26360,#18844,#18845);
#16054=AXIS2_PLACEMENT_3D('',#26361,#18846,#18847);
#16055=AXIS2_PLACEMENT_3D('',#26372,#18849,#18850);
#16056=AXIS2_PLACEMENT_3D('',#26383,#18852,#18853);
#16057=AXIS2_PLACEMENT_3D('',#26389,#18854,#18855);
#16058=AXIS2_PLACEMENT_3D('',#26393,#18856,#18857);
#16059=AXIS2_PLACEMENT_3D('',#26400,#18860,#18861);
#16060=AXIS2_PLACEMENT_3D('',#26402,#18863,#18864);
#16061=AXIS2_PLACEMENT_3D('',#26408,#18866,#18867);
#16062=AXIS2_PLACEMENT_3D('',#26419,#18869,#18870);
#16063=AXIS2_PLACEMENT_3D('',#26430,#18872,#18873);
#16064=AXIS2_PLACEMENT_3D('',#26436,#18874,#18875);
#16065=AXIS2_PLACEMENT_3D('',#26440,#18876,#18877);
#16066=AXIS2_PLACEMENT_3D('',#26447,#18880,#18881);
#16067=AXIS2_PLACEMENT_3D('',#26449,#18883,#18884);
#16068=AXIS2_PLACEMENT_3D('',#26455,#18886,#18887);
#16069=AXIS2_PLACEMENT_3D('',#26466,#18889,#18890);
#16070=AXIS2_PLACEMENT_3D('',#26477,#18892,#18893);
#16071=AXIS2_PLACEMENT_3D('',#26483,#18894,#18895);
#16072=AXIS2_PLACEMENT_3D('',#26487,#18896,#18897);
#16073=AXIS2_PLACEMENT_3D('',#26494,#18900,#18901);
#16074=AXIS2_PLACEMENT_3D('',#26496,#18903,#18904);
#16075=AXIS2_PLACEMENT_3D('',#26502,#18906,#18907);
#16076=AXIS2_PLACEMENT_3D('',#26513,#18909,#18910);
#16077=AXIS2_PLACEMENT_3D('',#26524,#18912,#18913);
#16078=AXIS2_PLACEMENT_3D('',#26530,#18914,#18915);
#16079=AXIS2_PLACEMENT_3D('',#26534,#18916,#18917);
#16080=AXIS2_PLACEMENT_3D('',#26541,#18920,#18921);
#16081=AXIS2_PLACEMENT_3D('',#26543,#18923,#18924);
#16082=AXIS2_PLACEMENT_3D('',#26549,#18926,#18927);
#16083=AXIS2_PLACEMENT_3D('',#26560,#18929,#18930);
#16084=AXIS2_PLACEMENT_3D('',#26571,#18932,#18933);
#16085=AXIS2_PLACEMENT_3D('',#26577,#18934,#18935);
#16086=AXIS2_PLACEMENT_3D('',#26581,#18936,#18937);
#16087=AXIS2_PLACEMENT_3D('',#26584,#18940,#18941);
#16088=AXIS2_PLACEMENT_3D('',#26590,#18943,#18944);
#16089=AXIS2_PLACEMENT_3D('',#26599,#18945,#18946);
#16090=AXIS2_PLACEMENT_3D('',#26600,#18947,#18948);
#16091=AXIS2_PLACEMENT_3D('',#26609,#18953,#18954);
#16092=AXIS2_PLACEMENT_3D('',#26615,#18958,#18959);
#16093=AXIS2_PLACEMENT_3D('',#26622,#18961,#18962);
#16094=AXIS2_PLACEMENT_3D('',#26633,#18964,#18965);
#16095=AXIS2_PLACEMENT_3D('',#26639,#18966,#18967);
#16096=AXIS2_PLACEMENT_3D('',#26643,#18968,#18969);
#16097=AXIS2_PLACEMENT_3D('',#26646,#18972,#18973);
#16098=AXIS2_PLACEMENT_3D('',#26652,#18975,#18976);
#16099=AXIS2_PLACEMENT_3D('',#26653,#18977,#18978);
#16100=AXIS2_PLACEMENT_3D('',#26654,#18979,#18980);
#16101=AXIS2_PLACEMENT_3D('',#26656,#18981,#18982);
#16102=AXIS2_PLACEMENT_3D('',#26659,#18984,#18985);
#16103=AXIS2_PLACEMENT_3D('',#26660,#18986,#18987);
#16104=AXIS2_PLACEMENT_3D('',#26663,#18989,#18990);
#16105=AXIS2_PLACEMENT_3D('',#26664,#18991,#18992);
#16106=AXIS2_PLACEMENT_3D('',#26666,#18994,#18995);
#16107=AXIS2_PLACEMENT_3D('',#26667,#18996,#18997);
#16108=AXIS2_PLACEMENT_3D('',#26668,#18998,#18999);
#16109=AXIS2_PLACEMENT_3D('',#26669,#19000,#19001);
#16110=AXIS2_PLACEMENT_3D('',#26670,#19002,#19003);
#16111=AXIS2_PLACEMENT_3D('',#26671,#19004,#19005);
#16112=AXIS2_PLACEMENT_3D('',#26672,#19006,#19007);
#16113=AXIS2_PLACEMENT_3D('',#26673,#19008,#19009);
#16114=AXIS2_PLACEMENT_3D('',#26674,#19010,#19011);
#16115=AXIS2_PLACEMENT_3D('',#26676,#19012,#19013);
#16116=AXIS2_PLACEMENT_3D('',#26678,#19015,#19016);
#16117=AXIS2_PLACEMENT_3D('',#26679,#19017,#19018);
#16118=AXIS2_PLACEMENT_3D('',#26682,#19019,#19020);
#16119=AXIS2_PLACEMENT_3D('',#26688,#19024,#19025);
#16120=AXIS2_PLACEMENT_3D('',#26694,#19029,#19030);
#16121=AXIS2_PLACEMENT_3D('',#26700,#19034,#19035);
#16122=AXIS2_PLACEMENT_3D('',#26701,#19036,#19037);
#16123=AXIS2_PLACEMENT_3D('',#26703,#19039,#19040);
#16124=AXIS2_PLACEMENT_3D('',#26704,#19041,#19042);
#16125=AXIS2_PLACEMENT_3D('',#26705,#19043,#19044);
#16126=AXIS2_PLACEMENT_3D('',#26706,#19045,#19046);
#16127=AXIS2_PLACEMENT_3D('',#26707,#19047,#19048);
#16128=AXIS2_PLACEMENT_3D('',#26708,#19049,#19050);
#16129=AXIS2_PLACEMENT_3D('',#26709,#19051,#19052);
#16130=AXIS2_PLACEMENT_3D('',#26710,#19053,#19054);
#16131=AXIS2_PLACEMENT_3D('',#26711,#19055,#19056);
#16132=AXIS2_PLACEMENT_3D('',#26712,#19057,#19058);
#16133=AXIS2_PLACEMENT_3D('',#26713,#19059,#19060);
#16134=AXIS2_PLACEMENT_3D('',#26714,#19061,#19062);
#16135=AXIS2_PLACEMENT_3D('',#26715,#19063,#19064);
#16136=AXIS2_PLACEMENT_3D('',#26719,#19065,#19066);
#16137=AXIS2_PLACEMENT_3D('',#26720,#19067,#19068);
#16138=AXIS2_PLACEMENT_3D('',#26722,#19069,#19070);
#16139=AXIS2_PLACEMENT_3D('',#26723,#19071,#19072);
#16140=AXIS2_PLACEMENT_3D('',#26725,#19073,#19074);
#16141=AXIS2_PLACEMENT_3D('',#26727,#19076,#19077);
#16142=AXIS2_PLACEMENT_3D('',#26729,#19078,#19079);
#16143=AXIS2_PLACEMENT_3D('',#26730,#19080,#19081);
#16144=AXIS2_PLACEMENT_3D('',#26732,#19082,#19083);
#16145=AXIS2_PLACEMENT_3D('',#26734,#19085,#19086);
#16146=AXIS2_PLACEMENT_3D('',#26736,#19087,#19088);
#16147=AXIS2_PLACEMENT_3D('',#26737,#19089,#19090);
#16148=AXIS2_PLACEMENT_3D('',#26739,#19091,#19092);
#16149=AXIS2_PLACEMENT_3D('',#26741,#19094,#19095);
#16150=AXIS2_PLACEMENT_3D('',#26743,#19096,#19097);
#16151=AXIS2_PLACEMENT_3D('',#26745,#19099,#19100);
#16152=AXIS2_PLACEMENT_3D('',#26746,#19101,#19102);
#16153=AXIS2_PLACEMENT_3D('',#26747,#19103,#19104);
#16154=AXIS2_PLACEMENT_3D('',#26760,#19111,#19112);
#16155=AXIS2_PLACEMENT_3D('',#26766,#19116,#19117);
#16156=AXIS2_PLACEMENT_3D('',#26774,#19122,#19123);
#16157=AXIS2_PLACEMENT_3D('',#26782,#19128,#19129);
#16158=AXIS2_PLACEMENT_3D('',#26792,#19135,#19136);
#16159=AXIS2_PLACEMENT_3D('',#26798,#19140,#19141);
#16160=AXIS2_PLACEMENT_3D('',#26806,#19146,#19147);
#16161=AXIS2_PLACEMENT_3D('',#26811,#19151,#19152);
#16162=AXIS2_PLACEMENT_3D('',#26815,#19155,#19156);
#16163=AXIS2_PLACEMENT_3D('',#26823,#19161,#19162);
#16164=AXIS2_PLACEMENT_3D('',#26828,#19166,#19167);
#16165=AXIS2_PLACEMENT_3D('',#26832,#19170,#19171);
#16166=AXIS2_PLACEMENT_3D('',#26838,#19175,#19176);
#16167=AXIS2_PLACEMENT_3D('',#26840,#19178,#19179);
#16168=AXIS2_PLACEMENT_3D('',#26842,#19181,#19182);
#16169=AXIS2_PLACEMENT_3D('',#26843,#19183,#19184);
#16170=AXIS2_PLACEMENT_3D('',#26844,#19185,#19186);
#16171=AXIS2_PLACEMENT_3D('',#26845,#19187,#19188);
#16172=AXIS2_PLACEMENT_3D('',#26846,#19189,#19190);
#16173=AXIS2_PLACEMENT_3D('',#26848,#19191,#19192);
#16174=AXIS2_PLACEMENT_3D('',#26851,#19194,#19195);
#16175=AXIS2_PLACEMENT_3D('',#26852,#19196,#19197);
#16176=AXIS2_PLACEMENT_3D('',#26854,#19198,#19199);
#16177=AXIS2_PLACEMENT_3D('',#26855,#19200,#19201);
#16178=AXIS2_PLACEMENT_3D('',#26858,#19203,#19204);
#16179=AXIS2_PLACEMENT_3D('',#26859,#19205,#19206);
#16180=AXIS2_PLACEMENT_3D('',#26861,#19207,#19208);
#16181=AXIS2_PLACEMENT_3D('',#26862,#19209,#19210);
#16182=AXIS2_PLACEMENT_3D('',#26864,#19211,#19212);
#16183=AXIS2_PLACEMENT_3D('',#26866,#19214,#19215);
#16184=AXIS2_PLACEMENT_3D('',#26868,#19216,#19217);
#16185=AXIS2_PLACEMENT_3D('',#26870,#19219,#19220);
#16186=AXIS2_PLACEMENT_3D('',#26872,#19221,#19222);
#16187=AXIS2_PLACEMENT_3D('',#26874,#19224,#19225);
#16188=AXIS2_PLACEMENT_3D('',#26876,#19226,#19227);
#16189=AXIS2_PLACEMENT_3D('',#26877,#19228,#19229);
#16190=AXIS2_PLACEMENT_3D('',#26880,#19231,#19232);
#16191=AXIS2_PLACEMENT_3D('',#26881,#19233,#19234);
#16192=AXIS2_PLACEMENT_3D('',#26883,#19235,#19236);
#16193=AXIS2_PLACEMENT_3D('',#26884,#19237,#19238);
#16194=AXIS2_PLACEMENT_3D('',#26886,#19239,#19240);
#16195=AXIS2_PLACEMENT_3D('',#26888,#19242,#19243);
#16196=AXIS2_PLACEMENT_3D('',#26890,#19244,#19245);
#16197=AXIS2_PLACEMENT_3D('',#26891,#19246,#19247);
#16198=AXIS2_PLACEMENT_3D('',#26894,#19249,#19250);
#16199=AXIS2_PLACEMENT_3D('',#26895,#19251,#19252);
#16200=AXIS2_PLACEMENT_3D('',#26898,#19254,#19255);
#16201=AXIS2_PLACEMENT_3D('',#26899,#19256,#19257);
#16202=AXIS2_PLACEMENT_3D('',#26902,#19259,#19260);
#16203=AXIS2_PLACEMENT_3D('',#26903,#19261,#19262);
#16204=AXIS2_PLACEMENT_3D('',#26904,#19263,#19264);
#16205=AXIS2_PLACEMENT_3D('',#26905,#19265,#19266);
#16206=AXIS2_PLACEMENT_3D('',#26907,#19267,#19268);
#16207=AXIS2_PLACEMENT_3D('',#26910,#19270,#19271);
#16208=AXIS2_PLACEMENT_3D('',#26911,#19272,#19273);
#16209=AXIS2_PLACEMENT_3D('',#26913,#19274,#19275);
#16210=AXIS2_PLACEMENT_3D('',#26914,#19276,#19277);
#16211=AXIS2_PLACEMENT_3D('',#26916,#19278,#19279);
#16212=AXIS2_PLACEMENT_3D('',#26917,#19280,#19281);
#16213=AXIS2_PLACEMENT_3D('',#26919,#19282,#19283);
#16214=AXIS2_PLACEMENT_3D('',#26921,#19285,#19286);
#16215=AXIS2_PLACEMENT_3D('',#26923,#19287,#19288);
#16216=AXIS2_PLACEMENT_3D('',#26926,#19290,#19291);
#16217=AXIS2_PLACEMENT_3D('',#26927,#19292,#19293);
#16218=AXIS2_PLACEMENT_3D('',#26929,#19294,#19295);
#16219=AXIS2_PLACEMENT_3D('',#26930,#19296,#19297);
#16220=AXIS2_PLACEMENT_3D('',#26932,#19298,#19299);
#16221=AXIS2_PLACEMENT_3D('',#26934,#19301,#19302);
#16222=AXIS2_PLACEMENT_3D('',#26936,#19303,#19304);
#16223=AXIS2_PLACEMENT_3D('',#26937,#19305,#19306);
#16224=AXIS2_PLACEMENT_3D('',#26940,#19308,#19309);
#16225=AXIS2_PLACEMENT_3D('',#26941,#19310,#19311);
#16226=AXIS2_PLACEMENT_3D('',#26942,#19312,#19313);
#16227=AXIS2_PLACEMENT_3D('',#26945,#19315,#19316);
#16228=AXIS2_PLACEMENT_3D('',#26946,#19317,#19318);
#16229=AXIS2_PLACEMENT_3D('',#26947,#19319,#19320);
#16230=AXIS2_PLACEMENT_3D('',#26948,#19321,#19322);
#16231=AXIS2_PLACEMENT_3D('',#26951,#19323,#19324);
#16232=AXIS2_PLACEMENT_3D('',#26952,#19325,#19326);
#16233=AXIS2_PLACEMENT_3D('',#26955,#19328,#19329);
#16234=AXIS2_PLACEMENT_3D('',#26956,#19330,#19331);
#16235=AXIS2_PLACEMENT_3D('',#26958,#19332,#19333);
#16236=AXIS2_PLACEMENT_3D('',#26959,#19334,#19335);
#16237=AXIS2_PLACEMENT_3D('',#26962,#19337,#19338);
#16238=AXIS2_PLACEMENT_3D('',#26963,#19339,#19340);
#16239=AXIS2_PLACEMENT_3D('',#26966,#19341,#19342);
#16240=AXIS2_PLACEMENT_3D('',#26967,#19343,#19344);
#16241=AXIS2_PLACEMENT_3D('',#26970,#19346,#19347);
#16242=AXIS2_PLACEMENT_3D('',#26971,#19348,#19349);
#16243=AXIS2_PLACEMENT_3D('',#26973,#19350,#19351);
#16244=AXIS2_PLACEMENT_3D('',#26974,#19352,#19353);
#16245=AXIS2_PLACEMENT_3D('',#26976,#19354,#19355);
#16246=AXIS2_PLACEMENT_3D('',#26978,#19357,#19358);
#16247=AXIS2_PLACEMENT_3D('',#26980,#19359,#19360);
#16248=AXIS2_PLACEMENT_3D('',#26982,#19362,#19363);
#16249=AXIS2_PLACEMENT_3D('',#26984,#19364,#19365);
#16250=AXIS2_PLACEMENT_3D('',#26985,#19366,#19367);
#16251=AXIS2_PLACEMENT_3D('',#26987,#19369,#19370);
#16252=AXIS2_PLACEMENT_3D('',#26989,#19371,#19372);
#16253=AXIS2_PLACEMENT_3D('',#26990,#19373,#19374);
#16254=AXIS2_PLACEMENT_3D('',#26992,#19376,#19377);
#16255=AXIS2_PLACEMENT_3D('',#26993,#19378,#19379);
#16256=AXIS2_PLACEMENT_3D('',#26995,#19380,#19381);
#16257=AXIS2_PLACEMENT_3D('',#26998,#19383,#19384);
#16258=AXIS2_PLACEMENT_3D('',#26999,#19385,#19386);
#16259=AXIS2_PLACEMENT_3D('',#27001,#19387,#19388);
#16260=AXIS2_PLACEMENT_3D('',#27003,#19390,#19391);
#16261=AXIS2_PLACEMENT_3D('',#27005,#19392,#19393);
#16262=AXIS2_PLACEMENT_3D('',#27006,#19394,#19395);
#16263=AXIS2_PLACEMENT_3D('',#27009,#19396,#19397);
#16264=AXIS2_PLACEMENT_3D('',#27012,#19399,#19400);
#16265=AXIS2_PLACEMENT_3D('',#27013,#19401,#19402);
#16266=AXIS2_PLACEMENT_3D('',#27014,#19403,#19404);
#16267=AXIS2_PLACEMENT_3D('',#27015,#19405,#19406);
#16268=AXIS2_PLACEMENT_3D('',#27017,#19407,#19408);
#16269=AXIS2_PLACEMENT_3D('',#27021,#19410,#19411);
#16270=AXIS2_PLACEMENT_3D('',#27022,#19412,#19413);
#16271=AXIS2_PLACEMENT_3D('',#27023,#19414,#19415);
#16272=AXIS2_PLACEMENT_3D('',#27025,#19416,#19417);
#16273=AXIS2_PLACEMENT_3D('',#27026,#19418,#19419);
#16274=AXIS2_PLACEMENT_3D('',#27028,#19420,#19421);
#16275=AXIS2_PLACEMENT_3D('',#27030,#19423,#19424);
#16276=AXIS2_PLACEMENT_3D('',#27032,#19425,#19426);
#16277=AXIS2_PLACEMENT_3D('',#27034,#19428,#19429);
#16278=AXIS2_PLACEMENT_3D('',#27081,#19431,#19432);
#16279=AXIS2_PLACEMENT_3D('',#27082,#19433,#19434);
#16280=AXIS2_PLACEMENT_3D('',#27083,#19435,#19436);
#16281=AXIS2_PLACEMENT_3D('',#27085,#19437,#19438);
#16282=AXIS2_PLACEMENT_3D('',#27088,#19440,#19441);
#16283=AXIS2_PLACEMENT_3D('',#27089,#19442,#19443);
#16284=AXIS2_PLACEMENT_3D('',#27091,#19444,#19445);
#16285=AXIS2_PLACEMENT_3D('',#27092,#19446,#19447);
#16286=AXIS2_PLACEMENT_3D('',#27094,#19448,#19449);
#16287=AXIS2_PLACEMENT_3D('',#27096,#19451,#19452);
#16288=AXIS2_PLACEMENT_3D('',#27098,#19453,#19454);
#16289=AXIS2_PLACEMENT_3D('',#27100,#19456,#19457);
#16290=AXIS2_PLACEMENT_3D('',#27102,#19458,#19459);
#16291=AXIS2_PLACEMENT_3D('',#27103,#19460,#19461);
#16292=AXIS2_PLACEMENT_3D('',#27105,#19462,#19463);
#16293=AXIS2_PLACEMENT_3D('',#27107,#19465,#19466);
#16294=AXIS2_PLACEMENT_3D('',#27109,#19467,#19468);
#16295=AXIS2_PLACEMENT_3D('',#27110,#19469,#19470);
#16296=AXIS2_PLACEMENT_3D('',#27113,#19471,#19472);
#16297=AXIS2_PLACEMENT_3D('',#27115,#19473,#19474);
#16298=AXIS2_PLACEMENT_3D('',#27117,#19475,#19476);
#16299=AXIS2_PLACEMENT_3D('',#27118,#19477,#19478);
#16300=AXIS2_PLACEMENT_3D('',#27120,#19479,#19480);
#16301=AXIS2_PLACEMENT_3D('',#27121,#19481,#19482);
#16302=AXIS2_PLACEMENT_3D('',#27124,#19484,#19485);
#16303=AXIS2_PLACEMENT_3D('',#27125,#19486,#19487);
#16304=AXIS2_PLACEMENT_3D('',#27126,#19488,#19489);
#16305=AXIS2_PLACEMENT_3D('',#27127,#19490,#19491);
#16306=AXIS2_PLACEMENT_3D('',#27129,#19492,#19493);
#16307=AXIS2_PLACEMENT_3D('',#27133,#19495,#19496);
#16308=AXIS2_PLACEMENT_3D('',#27134,#19497,#19498);
#16309=AXIS2_PLACEMENT_3D('',#27135,#19499,#19500);
#16310=AXIS2_PLACEMENT_3D('',#27138,#19501,#19502);
#16311=AXIS2_PLACEMENT_3D('',#27140,#19503,#19504);
#16312=AXIS2_PLACEMENT_3D('',#27142,#19505,#19506);
#16313=AXIS2_PLACEMENT_3D('',#27144,#19507,#19508);
#16314=AXIS2_PLACEMENT_3D('',#27146,#19509,#19510);
#16315=AXIS2_PLACEMENT_3D('',#27148,#19511,#19512);
#16316=AXIS2_PLACEMENT_3D('',#27150,#19513,#19514);
#16317=AXIS2_PLACEMENT_3D('',#27152,#19515,#19516);
#16318=AXIS2_PLACEMENT_3D('',#27154,#19517,#19518);
#16319=AXIS2_PLACEMENT_3D('',#27156,#19519,#19520);
#16320=AXIS2_PLACEMENT_3D('',#27158,#19521,#19522);
#16321=AXIS2_PLACEMENT_3D('',#27160,#19523,#19524);
#16322=AXIS2_PLACEMENT_3D('',#27162,#19525,#19526);
#16323=AXIS2_PLACEMENT_3D('',#27163,#19527,#19528);
#16324=AXIS2_PLACEMENT_3D('',#27164,#19529,#19530);
#16325=AXIS2_PLACEMENT_3D('',#27167,#19532,#19533);
#16326=AXIS2_PLACEMENT_3D('',#27168,#19534,#19535);
#16327=AXIS2_PLACEMENT_3D('',#27171,#19536,#19537);
#16328=AXIS2_PLACEMENT_3D('',#27174,#19540,#19541);
#16329=AXIS2_PLACEMENT_3D('',#27176,#19542,#19543);
#16330=AXIS2_PLACEMENT_3D('',#27178,#19545,#19546);
#16331=AXIS2_PLACEMENT_3D('',#27180,#19547,#19548);
#16332=AXIS2_PLACEMENT_3D('',#27182,#19550,#19551);
#16333=AXIS2_PLACEMENT_3D('',#27184,#19552,#19553);
#16334=AXIS2_PLACEMENT_3D('',#27186,#19555,#19556);
#16335=AXIS2_PLACEMENT_3D('',#27188,#19557,#19558);
#16336=AXIS2_PLACEMENT_3D('',#27190,#19560,#19561);
#16337=AXIS2_PLACEMENT_3D('',#27192,#19562,#19563);
#16338=AXIS2_PLACEMENT_3D('',#27194,#19565,#19566);
#16339=AXIS2_PLACEMENT_3D('',#27196,#19567,#19568);
#16340=AXIS2_PLACEMENT_3D('',#27198,#19570,#19571);
#16341=AXIS2_PLACEMENT_3D('',#27200,#19572,#19573);
#16342=AXIS2_PLACEMENT_3D('',#27202,#19575,#19576);
#16343=AXIS2_PLACEMENT_3D('',#27204,#19577,#19578);
#16344=AXIS2_PLACEMENT_3D('',#27206,#19580,#19581);
#16345=AXIS2_PLACEMENT_3D('',#27208,#19582,#19583);
#16346=AXIS2_PLACEMENT_3D('',#27210,#19585,#19586);
#16347=AXIS2_PLACEMENT_3D('',#27212,#19587,#19588);
#16348=AXIS2_PLACEMENT_3D('',#27214,#19590,#19591);
#16349=AXIS2_PLACEMENT_3D('',#27216,#19592,#19593);
#16350=AXIS2_PLACEMENT_3D('',#27218,#19595,#19596);
#16351=AXIS2_PLACEMENT_3D('',#27220,#19597,#19598);
#16352=AXIS2_PLACEMENT_3D('',#27222,#19600,#19601);
#16353=AXIS2_PLACEMENT_3D('',#27224,#19602,#19603);
#16354=AXIS2_PLACEMENT_3D('',#27225,#19604,#19605);
#16355=AXIS2_PLACEMENT_3D('',#27226,#19606,#19607);
#16356=AXIS2_PLACEMENT_3D('',#27227,#19608,#19609);
#16357=AXIS2_PLACEMENT_3D('',#27229,#19611,#19612);
#16358=AXIS2_PLACEMENT_3D('',#27230,#19613,#19614);
#16359=AXIS2_PLACEMENT_3D('',#27252,#19616,#19617);
#16360=AXIS2_PLACEMENT_3D('',#27263,#19618,#19619);
#16361=AXIS2_PLACEMENT_3D('',#27347,#19621,#19622);
#16362=AXIS2_PLACEMENT_3D('',#27437,#19624,#19625);
#16363=AXIS2_PLACEMENT_3D('',#27521,#19627,#19628);
#16364=AXIS2_PLACEMENT_3D('',#27611,#19630,#19631);
#16365=AXIS2_PLACEMENT_3D('',#27701,#19633,#19634);
#16366=AXIS2_PLACEMENT_3D('',#27785,#19636,#19637);
#16367=AXIS2_PLACEMENT_3D('',#27875,#19639,#19640);
#16368=AXIS2_PLACEMENT_3D('',#27959,#19642,#19643);
#16369=AXIS2_PLACEMENT_3D('',#28049,#19645,#19646);
#16370=AXIS2_PLACEMENT_3D('',#28133,#19648,#19649);
#16371=AXIS2_PLACEMENT_3D('',#28223,#19651,#19652);
#16372=AXIS2_PLACEMENT_3D('',#28310,#19654,#19655);
#16373=AXIS2_PLACEMENT_3D('',#28397,#19657,#19658);
#16374=AXIS2_PLACEMENT_3D('',#28487,#19660,#19661);
#16375=AXIS2_PLACEMENT_3D('',#28571,#19663,#19664);
#16376=AXIS2_PLACEMENT_3D('',#28661,#19666,#19667);
#16377=AXIS2_PLACEMENT_3D('',#28745,#19669,#19670);
#16378=AXIS2_PLACEMENT_3D('',#28835,#19672,#19673);
#16379=AXIS2_PLACEMENT_3D('',#28919,#19675,#19676);
#16380=AXIS2_PLACEMENT_3D('',#29006,#19678,#19679);
#16381=AXIS2_PLACEMENT_3D('',#29096,#19681,#19682);
#16382=AXIS2_PLACEMENT_3D('',#29180,#19684,#19685);
#16383=AXIS2_PLACEMENT_3D('',#29270,#19687,#19688);
#16384=AXIS2_PLACEMENT_3D('',#29354,#19690,#19691);
#16385=AXIS2_PLACEMENT_3D('',#29444,#19693,#19694);
#16386=AXIS2_PLACEMENT_3D('',#29528,#19696,#19697);
#16387=AXIS2_PLACEMENT_3D('',#29618,#19699,#19700);
#16388=AXIS2_PLACEMENT_3D('',#29708,#19702,#19703);
#16389=AXIS2_PLACEMENT_3D('',#29792,#19705,#19706);
#16390=AXIS2_PLACEMENT_3D('',#29882,#19708,#19709);
#16391=AXIS2_PLACEMENT_3D('',#29966,#19711,#19712);
#16392=AXIS2_PLACEMENT_3D('',#30056,#19714,#19715);
#16393=AXIS2_PLACEMENT_3D('',#30140,#19717,#19718);
#16394=AXIS2_PLACEMENT_3D('',#30155,#19720,#19721);
#16395=AXIS2_PLACEMENT_3D('',#30162,#19722,#19723);
#16396=AXIS2_PLACEMENT_3D('',#30199,#19725,#19726);
#16397=AXIS2_PLACEMENT_3D('',#30236,#19728,#19729);
#16398=AXIS2_PLACEMENT_3D('',#30273,#19731,#19732);
#16399=AXIS2_PLACEMENT_3D('',#30310,#19734,#19735);
#16400=AXIS2_PLACEMENT_3D('',#30347,#19737,#19738);
#16401=AXIS2_PLACEMENT_3D('',#30384,#19740,#19741);
#16402=AXIS2_PLACEMENT_3D('',#30422,#19743,#19744);
#16403=AXIS2_PLACEMENT_3D('',#30459,#19746,#19747);
#16404=AXIS2_PLACEMENT_3D('',#30496,#19749,#19750);
#16405=AXIS2_PLACEMENT_3D('',#30533,#19752,#19753);
#16406=AXIS2_PLACEMENT_3D('',#30570,#19755,#19756);
#16407=AXIS2_PLACEMENT_3D('',#30607,#19758,#19759);
#16408=AXIS2_PLACEMENT_3D('',#30644,#19761,#19762);
#16409=AXIS2_PLACEMENT_3D('',#30682,#19764,#19765);
#16410=AXIS2_PLACEMENT_3D('',#30718,#19767,#19768);
#16411=AXIS2_PLACEMENT_3D('',#30756,#19770,#19771);
#16412=AXIS2_PLACEMENT_3D('',#30793,#19773,#19774);
#16413=AXIS2_PLACEMENT_3D('',#30830,#19776,#19777);
#16414=AXIS2_PLACEMENT_3D('',#30867,#19779,#19780);
#16415=AXIS2_PLACEMENT_3D('',#30904,#19782,#19783);
#16416=AXIS2_PLACEMENT_3D('',#30942,#19785,#19786);
#16417=AXIS2_PLACEMENT_3D('',#30978,#19788,#19789);
#16418=AXIS2_PLACEMENT_3D('',#31016,#19791,#19792);
#16419=AXIS2_PLACEMENT_3D('',#31053,#19794,#19795);
#16420=AXIS2_PLACEMENT_3D('',#31090,#19797,#19798);
#16421=AXIS2_PLACEMENT_3D('',#31127,#19800,#19801);
#16422=AXIS2_PLACEMENT_3D('',#31164,#19803,#19804);
#16423=AXIS2_PLACEMENT_3D('',#31201,#19806,#19807);
#16424=AXIS2_PLACEMENT_3D('',#31238,#19809,#19810);
#16425=AXIS2_PLACEMENT_3D('',#31276,#19812,#19813);
#16426=AXIS2_PLACEMENT_3D('',#31313,#19815,#19816);
#16427=AXIS2_PLACEMENT_3D('',#31350,#19818,#19819);
#16428=AXIS2_PLACEMENT_3D('',#33401,#19821,#19822);
#16429=AXIS2_PLACEMENT_3D('',#33403,#19823,#19824);
#16430=AXIS2_PLACEMENT_3D('',#33404,#19825,#19826);
#16431=AXIS2_PLACEMENT_3D('',#33515,#19827,#19828);
#16432=AXIS2_PLACEMENT_3D('',#33516,#19829,#19830);
#16433=AXIS2_PLACEMENT_3D('',#35413,#19831,#19832);
#16434=AXIS2_PLACEMENT_3D('',#35422,#19837,#19838);
#16435=AXIS2_PLACEMENT_3D('',#35424,#19839,#19840);
#16436=AXIS2_PLACEMENT_3D('',#35426,#19842,#19843);
#16437=AXIS2_PLACEMENT_3D('',#35430,#19846,#19847);
#16438=AXIS2_PLACEMENT_3D('',#35431,#19848,#19849);
#16439=AXIS2_PLACEMENT_3D('',#35432,#19850,#19851);
#16440=AXIS2_PLACEMENT_3D('',#35441,#19856,#19857);
#16441=AXIS2_PLACEMENT_3D('',#35443,#19858,#19859);
#16442=AXIS2_PLACEMENT_3D('',#35445,#19861,#19862);
#16443=AXIS2_PLACEMENT_3D('',#35449,#19865,#19866);
#16444=AXIS2_PLACEMENT_3D('',#35450,#19867,#19868);
#16445=AXIS2_PLACEMENT_3D('',#35451,#19869,#19870);
#16446=AXIS2_PLACEMENT_3D('',#35460,#19875,#19876);
#16447=AXIS2_PLACEMENT_3D('',#35462,#19877,#19878);
#16448=AXIS2_PLACEMENT_3D('',#35464,#19880,#19881);
#16449=AXIS2_PLACEMENT_3D('',#35468,#19884,#19885);
#16450=AXIS2_PLACEMENT_3D('',#35469,#19886,#19887);
#16451=AXIS2_PLACEMENT_3D('',#35470,#19888,#19889);
#16452=AXIS2_PLACEMENT_3D('',#35479,#19894,#19895);
#16453=AXIS2_PLACEMENT_3D('',#35481,#19896,#19897);
#16454=AXIS2_PLACEMENT_3D('',#35483,#19899,#19900);
#16455=AXIS2_PLACEMENT_3D('',#35487,#19903,#19904);
#16456=AXIS2_PLACEMENT_3D('',#35488,#19905,#19906);
#16457=AXIS2_PLACEMENT_3D('',#35489,#19907,#19908);
#16458=AXIS2_PLACEMENT_3D('',#35498,#19913,#19914);
#16459=AXIS2_PLACEMENT_3D('',#35500,#19915,#19916);
#16460=AXIS2_PLACEMENT_3D('',#35502,#19918,#19919);
#16461=AXIS2_PLACEMENT_3D('',#35506,#19922,#19923);
#16462=AXIS2_PLACEMENT_3D('',#35507,#19924,#19925);
#16463=AXIS2_PLACEMENT_3D('',#35508,#19926,#19927);
#16464=AXIS2_PLACEMENT_3D('',#35517,#19932,#19933);
#16465=AXIS2_PLACEMENT_3D('',#35519,#19934,#19935);
#16466=AXIS2_PLACEMENT_3D('',#35521,#19937,#19938);
#16467=AXIS2_PLACEMENT_3D('',#35525,#19941,#19942);
#16468=AXIS2_PLACEMENT_3D('',#35526,#19943,#19944);
#16469=AXIS2_PLACEMENT_3D('',#35527,#19945,#19946);
#16470=AXIS2_PLACEMENT_3D('',#35536,#19951,#19952);
#16471=AXIS2_PLACEMENT_3D('',#35538,#19953,#19954);
#16472=AXIS2_PLACEMENT_3D('',#35540,#19956,#19957);
#16473=AXIS2_PLACEMENT_3D('',#35544,#19960,#19961);
#16474=AXIS2_PLACEMENT_3D('',#35545,#19962,#19963);
#16475=AXIS2_PLACEMENT_3D('',#35546,#19964,#19965);
#16476=AXIS2_PLACEMENT_3D('',#35555,#19970,#19971);
#16477=AXIS2_PLACEMENT_3D('',#35557,#19972,#19973);
#16478=AXIS2_PLACEMENT_3D('',#35559,#19975,#19976);
#16479=AXIS2_PLACEMENT_3D('',#35563,#19979,#19980);
#16480=AXIS2_PLACEMENT_3D('',#35564,#19981,#19982);
#16481=AXIS2_PLACEMENT_3D('',#35565,#19983,#19984);
#16482=AXIS2_PLACEMENT_3D('',#35574,#19989,#19990);
#16483=AXIS2_PLACEMENT_3D('',#35576,#19991,#19992);
#16484=AXIS2_PLACEMENT_3D('',#35578,#19994,#19995);
#16485=AXIS2_PLACEMENT_3D('',#35582,#19998,#19999);
#16486=AXIS2_PLACEMENT_3D('',#35583,#20000,#20001);
#16487=AXIS2_PLACEMENT_3D('',#35584,#20002,#20003);
#16488=AXIS2_PLACEMENT_3D('',#35593,#20008,#20009);
#16489=AXIS2_PLACEMENT_3D('',#35595,#20010,#20011);
#16490=AXIS2_PLACEMENT_3D('',#35597,#20013,#20014);
#16491=AXIS2_PLACEMENT_3D('',#35601,#20017,#20018);
#16492=AXIS2_PLACEMENT_3D('',#35602,#20019,#20020);
#16493=AXIS2_PLACEMENT_3D('',#35603,#20021,#20022);
#16494=AXIS2_PLACEMENT_3D('',#35612,#20027,#20028);
#16495=AXIS2_PLACEMENT_3D('',#35614,#20029,#20030);
#16496=AXIS2_PLACEMENT_3D('',#35616,#20032,#20033);
#16497=AXIS2_PLACEMENT_3D('',#35620,#20036,#20037);
#16498=AXIS2_PLACEMENT_3D('',#35621,#20038,#20039);
#16499=AXIS2_PLACEMENT_3D('',#35622,#20040,#20041);
#16500=AXIS2_PLACEMENT_3D('',#35631,#20046,#20047);
#16501=AXIS2_PLACEMENT_3D('',#35633,#20048,#20049);
#16502=AXIS2_PLACEMENT_3D('',#35635,#20051,#20052);
#16503=AXIS2_PLACEMENT_3D('',#35639,#20055,#20056);
#16504=AXIS2_PLACEMENT_3D('',#35640,#20057,#20058);
#16505=AXIS2_PLACEMENT_3D('',#35641,#20059,#20060);
#16506=AXIS2_PLACEMENT_3D('',#35650,#20065,#20066);
#16507=AXIS2_PLACEMENT_3D('',#35652,#20067,#20068);
#16508=AXIS2_PLACEMENT_3D('',#35654,#20070,#20071);
#16509=AXIS2_PLACEMENT_3D('',#35658,#20074,#20075);
#16510=AXIS2_PLACEMENT_3D('',#35659,#20076,#20077);
#16511=AXIS2_PLACEMENT_3D('',#35660,#20078,#20079);
#16512=AXIS2_PLACEMENT_3D('',#35669,#20084,#20085);
#16513=AXIS2_PLACEMENT_3D('',#35671,#20086,#20087);
#16514=AXIS2_PLACEMENT_3D('',#35673,#20089,#20090);
#16515=AXIS2_PLACEMENT_3D('',#35677,#20093,#20094);
#16516=AXIS2_PLACEMENT_3D('',#35678,#20095,#20096);
#16517=AXIS2_PLACEMENT_3D('',#35679,#20097,#20098);
#16518=AXIS2_PLACEMENT_3D('',#35688,#20103,#20104);
#16519=AXIS2_PLACEMENT_3D('',#35690,#20105,#20106);
#16520=AXIS2_PLACEMENT_3D('',#35692,#20108,#20109);
#16521=AXIS2_PLACEMENT_3D('',#35696,#20112,#20113);
#16522=AXIS2_PLACEMENT_3D('',#35697,#20114,#20115);
#16523=AXIS2_PLACEMENT_3D('',#35698,#20116,#20117);
#16524=AXIS2_PLACEMENT_3D('',#35707,#20122,#20123);
#16525=AXIS2_PLACEMENT_3D('',#35709,#20124,#20125);
#16526=AXIS2_PLACEMENT_3D('',#35711,#20127,#20128);
#16527=AXIS2_PLACEMENT_3D('',#35715,#20131,#20132);
#16528=AXIS2_PLACEMENT_3D('',#35716,#20133,#20134);
#16529=AXIS2_PLACEMENT_3D('',#35717,#20135,#20136);
#16530=AXIS2_PLACEMENT_3D('',#35726,#20141,#20142);
#16531=AXIS2_PLACEMENT_3D('',#35728,#20143,#20144);
#16532=AXIS2_PLACEMENT_3D('',#35730,#20146,#20147);
#16533=AXIS2_PLACEMENT_3D('',#35734,#20150,#20151);
#16534=AXIS2_PLACEMENT_3D('',#35735,#20152,#20153);
#16535=AXIS2_PLACEMENT_3D('',#35736,#20154,#20155);
#16536=AXIS2_PLACEMENT_3D('',#35745,#20160,#20161);
#16537=AXIS2_PLACEMENT_3D('',#35747,#20162,#20163);
#16538=AXIS2_PLACEMENT_3D('',#35750,#20165,#20166);
#16539=AXIS2_PLACEMENT_3D('',#35751,#20167,#20168);
#16540=AXIS2_PLACEMENT_3D('',#35755,#20171,#20172);
#16541=AXIS2_PLACEMENT_3D('',#35757,#20173,#20174);
#16542=AXIS2_PLACEMENT_3D('',#35758,#20175,#20176);
#16543=AXIS2_PLACEMENT_3D('',#35759,#20177,#20178);
#16544=AXIS2_PLACEMENT_3D('',#35768,#20183,#20184);
#16545=AXIS2_PLACEMENT_3D('',#35770,#20185,#20186);
#16546=AXIS2_PLACEMENT_3D('',#35772,#20188,#20189);
#16547=AXIS2_PLACEMENT_3D('',#35776,#20192,#20193);
#16548=AXIS2_PLACEMENT_3D('',#35777,#20194,#20195);
#16549=AXIS2_PLACEMENT_3D('',#35778,#20196,#20197);
#16550=AXIS2_PLACEMENT_3D('',#35787,#20202,#20203);
#16551=AXIS2_PLACEMENT_3D('',#35789,#20204,#20205);
#16552=AXIS2_PLACEMENT_3D('',#35791,#20207,#20208);
#16553=AXIS2_PLACEMENT_3D('',#35795,#20211,#20212);
#16554=AXIS2_PLACEMENT_3D('',#35796,#20213,#20214);
#16555=AXIS2_PLACEMENT_3D('',#35797,#20215,#20216);
#16556=AXIS2_PLACEMENT_3D('',#35806,#20221,#20222);
#16557=AXIS2_PLACEMENT_3D('',#35808,#20223,#20224);
#16558=AXIS2_PLACEMENT_3D('',#35810,#20226,#20227);
#16559=AXIS2_PLACEMENT_3D('',#35814,#20230,#20231);
#16560=AXIS2_PLACEMENT_3D('',#35815,#20232,#20233);
#16561=AXIS2_PLACEMENT_3D('',#35816,#20234,#20235);
#16562=AXIS2_PLACEMENT_3D('',#35825,#20240,#20241);
#16563=AXIS2_PLACEMENT_3D('',#35827,#20242,#20243);
#16564=AXIS2_PLACEMENT_3D('',#35829,#20245,#20246);
#16565=AXIS2_PLACEMENT_3D('',#35833,#20249,#20250);
#16566=AXIS2_PLACEMENT_3D('',#35834,#20251,#20252);
#16567=AXIS2_PLACEMENT_3D('',#35835,#20253,#20254);
#16568=AXIS2_PLACEMENT_3D('',#35844,#20259,#20260);
#16569=AXIS2_PLACEMENT_3D('',#35846,#20261,#20262);
#16570=AXIS2_PLACEMENT_3D('',#35848,#20264,#20265);
#16571=AXIS2_PLACEMENT_3D('',#35852,#20268,#20269);
#16572=AXIS2_PLACEMENT_3D('',#35853,#20270,#20271);
#16573=AXIS2_PLACEMENT_3D('',#35854,#20272,#20273);
#16574=AXIS2_PLACEMENT_3D('',#35863,#20278,#20279);
#16575=AXIS2_PLACEMENT_3D('',#35865,#20280,#20281);
#16576=AXIS2_PLACEMENT_3D('',#35867,#20283,#20284);
#16577=AXIS2_PLACEMENT_3D('',#35871,#20287,#20288);
#16578=AXIS2_PLACEMENT_3D('',#35872,#20289,#20290);
#16579=AXIS2_PLACEMENT_3D('',#35873,#20291,#20292);
#16580=AXIS2_PLACEMENT_3D('',#35882,#20297,#20298);
#16581=AXIS2_PLACEMENT_3D('',#35884,#20299,#20300);
#16582=AXIS2_PLACEMENT_3D('',#35886,#20302,#20303);
#16583=AXIS2_PLACEMENT_3D('',#35890,#20306,#20307);
#16584=AXIS2_PLACEMENT_3D('',#35891,#20308,#20309);
#16585=AXIS2_PLACEMENT_3D('',#35892,#20310,#20311);
#16586=AXIS2_PLACEMENT_3D('',#35901,#20316,#20317);
#16587=AXIS2_PLACEMENT_3D('',#35903,#20318,#20319);
#16588=AXIS2_PLACEMENT_3D('',#35905,#20321,#20322);
#16589=AXIS2_PLACEMENT_3D('',#35909,#20325,#20326);
#16590=AXIS2_PLACEMENT_3D('',#35910,#20327,#20328);
#16591=AXIS2_PLACEMENT_3D('',#35911,#20329,#20330);
#16592=AXIS2_PLACEMENT_3D('',#35920,#20335,#20336);
#16593=AXIS2_PLACEMENT_3D('',#35922,#20337,#20338);
#16594=AXIS2_PLACEMENT_3D('',#35924,#20340,#20341);
#16595=AXIS2_PLACEMENT_3D('',#35928,#20344,#20345);
#16596=AXIS2_PLACEMENT_3D('',#35929,#20346,#20347);
#16597=AXIS2_PLACEMENT_3D('',#35930,#20348,#20349);
#16598=AXIS2_PLACEMENT_3D('',#35939,#20354,#20355);
#16599=AXIS2_PLACEMENT_3D('',#35941,#20356,#20357);
#16600=AXIS2_PLACEMENT_3D('',#35943,#20359,#20360);
#16601=AXIS2_PLACEMENT_3D('',#35947,#20363,#20364);
#16602=AXIS2_PLACEMENT_3D('',#35948,#20365,#20366);
#16603=AXIS2_PLACEMENT_3D('',#35949,#20367,#20368);
#16604=AXIS2_PLACEMENT_3D('',#35958,#20373,#20374);
#16605=AXIS2_PLACEMENT_3D('',#35960,#20375,#20376);
#16606=AXIS2_PLACEMENT_3D('',#35962,#20378,#20379);
#16607=AXIS2_PLACEMENT_3D('',#35966,#20382,#20383);
#16608=AXIS2_PLACEMENT_3D('',#35967,#20384,#20385);
#16609=AXIS2_PLACEMENT_3D('',#35968,#20386,#20387);
#16610=AXIS2_PLACEMENT_3D('',#35977,#20392,#20393);
#16611=AXIS2_PLACEMENT_3D('',#35979,#20394,#20395);
#16612=AXIS2_PLACEMENT_3D('',#35981,#20397,#20398);
#16613=AXIS2_PLACEMENT_3D('',#35985,#20401,#20402);
#16614=AXIS2_PLACEMENT_3D('',#35986,#20403,#20404);
#16615=AXIS2_PLACEMENT_3D('',#35987,#20405,#20406);
#16616=AXIS2_PLACEMENT_3D('',#35996,#20411,#20412);
#16617=AXIS2_PLACEMENT_3D('',#35998,#20413,#20414);
#16618=AXIS2_PLACEMENT_3D('',#36000,#20416,#20417);
#16619=AXIS2_PLACEMENT_3D('',#36004,#20420,#20421);
#16620=AXIS2_PLACEMENT_3D('',#36005,#20422,#20423);
#16621=AXIS2_PLACEMENT_3D('',#36006,#20424,#20425);
#16622=AXIS2_PLACEMENT_3D('',#36015,#20430,#20431);
#16623=AXIS2_PLACEMENT_3D('',#36017,#20432,#20433);
#16624=AXIS2_PLACEMENT_3D('',#36019,#20435,#20436);
#16625=AXIS2_PLACEMENT_3D('',#36023,#20439,#20440);
#16626=AXIS2_PLACEMENT_3D('',#36024,#20441,#20442);
#16627=AXIS2_PLACEMENT_3D('',#36025,#20443,#20444);
#16628=AXIS2_PLACEMENT_3D('',#36034,#20449,#20450);
#16629=AXIS2_PLACEMENT_3D('',#36036,#20451,#20452);
#16630=AXIS2_PLACEMENT_3D('',#36038,#20454,#20455);
#16631=AXIS2_PLACEMENT_3D('',#36042,#20458,#20459);
#16632=AXIS2_PLACEMENT_3D('',#36043,#20460,#20461);
#16633=AXIS2_PLACEMENT_3D('',#36044,#20462,#20463);
#16634=AXIS2_PLACEMENT_3D('',#36053,#20468,#20469);
#16635=AXIS2_PLACEMENT_3D('',#36055,#20470,#20471);
#16636=AXIS2_PLACEMENT_3D('',#36057,#20473,#20474);
#16637=AXIS2_PLACEMENT_3D('',#36061,#20477,#20478);
#16638=AXIS2_PLACEMENT_3D('',#36062,#20479,#20480);
#16639=AXIS2_PLACEMENT_3D('',#36063,#20481,#20482);
#16640=AXIS2_PLACEMENT_3D('',#36072,#20487,#20488);
#16641=AXIS2_PLACEMENT_3D('',#36074,#20489,#20490);
#16642=AXIS2_PLACEMENT_3D('',#36076,#20492,#20493);
#16643=AXIS2_PLACEMENT_3D('',#36080,#20496,#20497);
#16644=AXIS2_PLACEMENT_3D('',#36081,#20498,#20499);
#16645=AXIS2_PLACEMENT_3D('',#36082,#20500,#20501);
#16646=AXIS2_PLACEMENT_3D('',#36091,#20506,#20507);
#16647=AXIS2_PLACEMENT_3D('',#36093,#20508,#20509);
#16648=AXIS2_PLACEMENT_3D('',#36095,#20511,#20512);
#16649=AXIS2_PLACEMENT_3D('',#36099,#20515,#20516);
#16650=AXIS2_PLACEMENT_3D('',#36100,#20517,#20518);
#16651=AXIS2_PLACEMENT_3D('',#36101,#20519,#20520);
#16652=AXIS2_PLACEMENT_3D('',#36110,#20525,#20526);
#16653=AXIS2_PLACEMENT_3D('',#36116,#20530,#20531);
#16654=AXIS2_PLACEMENT_3D('',#36122,#20535,#20536);
#16655=AXIS2_PLACEMENT_3D('',#36128,#20540,#20541);
#16656=AXIS2_PLACEMENT_3D('',#36134,#20545,#20546);
#16657=AXIS2_PLACEMENT_3D('',#36137,#20549,#20550);
#16658=AXIS2_PLACEMENT_3D('',#36138,#20551,#20552);
#16659=AXIS2_PLACEMENT_3D('',#36140,#20553,#20554);
#16660=AXIS2_PLACEMENT_3D('',#36141,#20555,#20556);
#16661=AXIS2_PLACEMENT_3D('',#36143,#20558,#20559);
#16662=AXIS2_PLACEMENT_3D('',#36144,#20560,#20561);
#16663=AXIS2_PLACEMENT_3D('',#36145,#20562,#20563);
#16664=AXIS2_PLACEMENT_3D('',#36147,#20564,#20565);
#16665=AXIS2_PLACEMENT_3D('',#36148,#20566,#20567);
#16666=AXIS2_PLACEMENT_3D('',#36150,#20568,#20569);
#16667=AXIS2_PLACEMENT_3D('',#36153,#20572,#20573);
#16668=AXIS2_PLACEMENT_3D('',#36155,#20574,#20575);
#16669=AXIS2_PLACEMENT_3D('',#36157,#20577,#20578);
#16670=AXIS2_PLACEMENT_3D('',#36158,#20579,#20580);
#16671=AXIS2_PLACEMENT_3D('',#36159,#20581,#20582);
#16672=AXIS2_PLACEMENT_3D('',#36181,#20584,#20585);
#16673=AXIS2_PLACEMENT_3D('',#36192,#20586,#20587);
#16674=AXIS2_PLACEMENT_3D('',#36282,#20589,#20590);
#16675=AXIS2_PLACEMENT_3D('',#36366,#20592,#20593);
#16676=AXIS2_PLACEMENT_3D('',#36456,#20595,#20596);
#16677=AXIS2_PLACEMENT_3D('',#36546,#20598,#20599);
#16678=AXIS2_PLACEMENT_3D('',#36636,#20601,#20602);
#16679=AXIS2_PLACEMENT_3D('',#36720,#20604,#20605);
#16680=AXIS2_PLACEMENT_3D('',#36730,#20607,#20608);
#16681=AXIS2_PLACEMENT_3D('',#36731,#20609,#20610);
#16682=AXIS2_PLACEMENT_3D('',#36752,#20612,#20613);
#16683=AXIS2_PLACEMENT_3D('',#36768,#20614,#20615);
#16684=AXIS2_PLACEMENT_3D('',#36805,#20617,#20618);
#16685=AXIS2_PLACEMENT_3D('',#36843,#20620,#20621);
#16686=AXIS2_PLACEMENT_3D('',#36881,#20623,#20624);
#16687=AXIS2_PLACEMENT_3D('',#36918,#20626,#20627);
#16688=AXIS2_PLACEMENT_3D('',#36955,#20629,#20630);
#16689=AXIS2_PLACEMENT_3D('',#36962,#20634,#20635);
#16690=AXIS2_PLACEMENT_3D('',#36968,#20639,#20640);
#16691=AXIS2_PLACEMENT_3D('',#36975,#20644,#20645);
#16692=AXIS2_PLACEMENT_3D('',#36981,#20649,#20650);
#16693=AXIS2_PLACEMENT_3D('',#36984,#20653,#20654);
#16694=AXIS2_PLACEMENT_3D('',#36991,#20658,#20659);
#16695=AXIS2_PLACEMENT_3D('',#36997,#20663,#20664);
#16696=AXIS2_PLACEMENT_3D('',#37004,#20668,#20669);
#16697=AXIS2_PLACEMENT_3D('',#37010,#20673,#20674);
#16698=AXIS2_PLACEMENT_3D('',#37013,#20677,#20678);
#16699=AXIS2_PLACEMENT_3D('',#37020,#20682,#20683);
#16700=AXIS2_PLACEMENT_3D('',#37026,#20687,#20688);
#16701=AXIS2_PLACEMENT_3D('',#37033,#20692,#20693);
#16702=AXIS2_PLACEMENT_3D('',#37039,#20697,#20698);
#16703=AXIS2_PLACEMENT_3D('',#37042,#20701,#20702);
#16704=AXIS2_PLACEMENT_3D('',#37045,#20705,#20706);
#16705=AXIS2_PLACEMENT_3D('',#37048,#20709,#20710);
#16706=AXIS2_PLACEMENT_3D('',#37051,#20713,#20714);
#16707=AXIS2_PLACEMENT_3D('',#37053,#20716,#20717);
#16708=AXIS2_PLACEMENT_3D('',#37055,#20719,#20720);
#16709=AXIS2_PLACEMENT_3D('',#37057,#20722,#20723);
#16710=AXIS2_PLACEMENT_3D('',#37070,#20730,#20731);
#16711=AXIS2_PLACEMENT_3D('',#37076,#20735,#20736);
#16712=AXIS2_PLACEMENT_3D('',#37080,#20739,#20740);
#16713=AXIS2_PLACEMENT_3D('',#37086,#20744,#20745);
#16714=AXIS2_PLACEMENT_3D('',#37090,#20748,#20749);
#16715=AXIS2_PLACEMENT_3D('',#37092,#20751,#20752);
#16716=AXIS2_PLACEMENT_3D('',#37094,#20754,#20755);
#16717=AXIS2_PLACEMENT_3D('',#37100,#20759,#20760);
#16718=AXIS2_PLACEMENT_3D('',#37104,#20763,#20764);
#16719=AXIS2_PLACEMENT_3D('',#37758,#20767,#20768);
#16720=AXIS2_PLACEMENT_3D('',#37760,#20769,#20770);
#16721=AXIS2_PLACEMENT_3D('',#37761,#20771,#20772);
#16722=AXIS2_PLACEMENT_3D('',#37881,#20773,#20774);
#16723=AXIS2_PLACEMENT_3D('',#37882,#20775,#20776);
#16724=AXIS2_PLACEMENT_3D('',#38405,#20777,#20778);
#16725=AXIS2_PLACEMENT_3D('',#38406,#20779,#20780);
#16726=AXIS2_PLACEMENT_3D('',#38408,#20781,#20782);
#16727=AXIS2_PLACEMENT_3D('',#38409,#20783,#20784);
#16728=AXIS2_PLACEMENT_3D('',#38413,#20787,#20788);
#16729=AXIS2_PLACEMENT_3D('',#38417,#20791,#20792);
#16730=AXIS2_PLACEMENT_3D('',#38419,#20794,#20795);
#16731=AXIS2_PLACEMENT_3D('',#38420,#20796,#20797);
#16732=AXIS2_PLACEMENT_3D('',#38422,#20799,#20800);
#16733=AXIS2_PLACEMENT_3D('',#38424,#20802,#20803);
#16734=AXIS2_PLACEMENT_3D('',#38426,#20805,#20806);
#16735=AXIS2_PLACEMENT_3D('',#38428,#20807,#20808);
#16736=AXIS2_PLACEMENT_3D('',#38429,#20809,#20810);
#16737=AXIS2_PLACEMENT_3D('',#38431,#20811,#20812);
#16738=AXIS2_PLACEMENT_3D('',#38433,#20813,#20814);
#16739=AXIS2_PLACEMENT_3D('',#38434,#20815,#20816);
#16740=AXIS2_PLACEMENT_3D('',#38436,#20818,#20819);
#16741=AXIS2_PLACEMENT_3D('',#38438,#20820,#20821);
#16742=AXIS2_PLACEMENT_3D('',#38439,#20822,#20823);
#16743=AXIS2_PLACEMENT_3D('',#38441,#20825,#20826);
#16744=AXIS2_PLACEMENT_3D('',#38442,#20827,#20828);
#16745=AXIS2_PLACEMENT_3D('',#38444,#20830,#20831);
#16746=AXIS2_PLACEMENT_3D('',#38445,#20832,#20833);
#16747=AXIS2_PLACEMENT_3D('',#38446,#20834,#20835);
#16748=AXIS2_PLACEMENT_3D('',#38447,#20836,#20837);
#16749=AXIS2_PLACEMENT_3D('',#38448,#20838,#20839);
#16750=AXIS2_PLACEMENT_3D('',#38449,#20840,#20841);
#16751=AXIS2_PLACEMENT_3D('',#38450,#20842,#20843);
#16752=AXIS2_PLACEMENT_3D('',#38451,#20844,#20845);
#16753=AXIS2_PLACEMENT_3D('',#38452,#20846,#20847);
#16754=AXIS2_PLACEMENT_3D('',#38453,#20848,#20849);
#16755=AXIS2_PLACEMENT_3D('',#38454,#20850,#20851);
#16756=AXIS2_PLACEMENT_3D('',#38455,#20852,#20853);
#16757=AXIS2_PLACEMENT_3D('',#38456,#20854,#20855);
#16758=AXIS2_PLACEMENT_3D('',#38457,#20856,#20857);
#16759=AXIS2_PLACEMENT_3D('',#38458,#20858,#20859);
#16760=AXIS2_PLACEMENT_3D('',#38459,#20860,#20861);
#16761=AXIS2_PLACEMENT_3D('',#38460,#20862,#20863);
#16762=AXIS2_PLACEMENT_3D('',#38461,#20864,#20865);
#16763=AXIS2_PLACEMENT_3D('',#38462,#20866,#20867);
#16764=AXIS2_PLACEMENT_3D('',#38463,#20868,#20869);
#16765=AXIS2_PLACEMENT_3D('',#38464,#20870,#20871);
#16766=AXIS2_PLACEMENT_3D('',#38465,#20872,#20873);
#16767=AXIS2_PLACEMENT_3D('',#38466,#20874,#20875);
#16768=AXIS2_PLACEMENT_3D('',#38467,#20876,#20877);
#16769=AXIS2_PLACEMENT_3D('',#38468,#20878,#20879);
#16770=AXIS2_PLACEMENT_3D('',#38469,#20880,#20881);
#16771=AXIS2_PLACEMENT_3D('',#38470,#20882,#20883);
#16772=AXIS2_PLACEMENT_3D('',#38471,#20884,#20885);
#16773=AXIS2_PLACEMENT_3D('',#38472,#20886,#20887);
#16774=AXIS2_PLACEMENT_3D('',#38473,#20888,#20889);
#16775=DIRECTION('axis',(0.,0.,1.));
#16776=DIRECTION('refdir',(1.,0.,0.));
#16777=DIRECTION('axis',(0.,0.,1.));
#16778=DIRECTION('refdir',(1.,0.,0.));
#16779=DIRECTION('center_axis',(0.,0.,1.));
#16780=DIRECTION('ref_axis',(1.,0.,0.));
#16781=DIRECTION('center_axis',(0.,0.,1.));
#16782=DIRECTION('ref_axis',(1.,0.,0.));
#16783=DIRECTION('',(-0.707106781186548,8.65956056235493E-17,0.707106781186548));
#16784=DIRECTION('center_axis',(0.,0.,-1.));
#16785=DIRECTION('ref_axis',(1.,0.,0.));
#16786=DIRECTION('center_axis',(0.,0.,-1.));
#16787=DIRECTION('ref_axis',(1.,0.,0.));
#16788=DIRECTION('',(0.,0.,1.));
#16789=DIRECTION('center_axis',(0.,0.,1.));
#16790=DIRECTION('ref_axis',(1.,0.,0.));
#16791=DIRECTION('center_axis',(0.,0.,1.));
#16792=DIRECTION('ref_axis',(1.,0.,0.));
#16793=DIRECTION('center_axis',(0.,0.,1.));
#16794=DIRECTION('ref_axis',(1.,0.,0.));
#16795=DIRECTION('center_axis',(0.,0.,1.));
#16796=DIRECTION('ref_axis',(1.,0.,0.));
#16797=DIRECTION('center_axis',(1.,0.,0.));
#16798=DIRECTION('ref_axis',(0.,0.,-1.));
#16799=DIRECTION('center_axis',(1.,0.,0.));
#16800=DIRECTION('ref_axis',(0.,0.,-1.));
#16801=DIRECTION('',(-0.707106781186548,8.65956056235493E-17,-0.707106781186548));
#16802=DIRECTION('center_axis',(-1.,0.,0.));
#16803=DIRECTION('ref_axis',(0.,0.,-1.));
#16804=DIRECTION('center_axis',(1.,0.,0.));
#16805=DIRECTION('ref_axis',(0.,0.,-1.));
#16806=DIRECTION('',(0.,-1.,0.));
#16807=DIRECTION('center_axis',(-1.,0.,0.));
#16808=DIRECTION('ref_axis',(0.,0.,-1.));
#16809=DIRECTION('',(0.,0.,1.));
#16810=DIRECTION('center_axis',(-1.,0.,0.));
#16811=DIRECTION('ref_axis',(0.,0.,1.));
#16812=DIRECTION('',(0.,1.,0.));
#16813=DIRECTION('center_axis',(-1.,0.,0.));
#16814=DIRECTION('ref_axis',(0.,-1.,1.83697019872103E-16));
#16815=DIRECTION('center_axis',(1.,0.,0.));
#16816=DIRECTION('ref_axis',(0.,0.,-1.));
#16817=DIRECTION('center_axis',(1.,0.,0.));
#16818=DIRECTION('ref_axis',(0.,0.,-1.));
#16819=DIRECTION('',(1.,0.,0.));
#16820=DIRECTION('center_axis',(0.,0.,-1.));
#16821=DIRECTION('ref_axis',(1.,0.,0.));
#16822=DIRECTION('center_axis',(0.,0.,-1.));
#16823=DIRECTION('ref_axis',(1.,0.,0.));
#16824=DIRECTION('',(-0.707106781186548,-8.65956056235493E-17,-0.707106781186548));
#16825=DIRECTION('center_axis',(0.,0.,1.));
#16826=DIRECTION('ref_axis',(1.,0.,0.));
#16827=DIRECTION('center_axis',(0.,0.,1.));
#16828=DIRECTION('ref_axis',(1.,0.,0.));
#16829=DIRECTION('center_axis',(0.,0.,1.));
#16830=DIRECTION('ref_axis',(1.,0.,0.));
#16831=DIRECTION('center_axis',(0.,0.,1.));
#16832=DIRECTION('ref_axis',(1.,0.,0.));
#16833=DIRECTION('',(0.,0.,-1.));
#16834=DIRECTION('center_axis',(0.,0.,-1.));
#16835=DIRECTION('ref_axis',(1.,0.,0.));
#16836=DIRECTION('center_axis',(0.,0.,-1.));
#16837=DIRECTION('ref_axis',(1.,0.,0.));
#16838=DIRECTION('center_axis',(1.,0.,0.));
#16839=DIRECTION('ref_axis',(0.,0.,-1.));
#16840=DIRECTION('center_axis',(1.,0.,0.));
#16841=DIRECTION('ref_axis',(0.,0.,-1.));
#16842=DIRECTION('',(-0.707106781186548,8.65956056235493E-17,-0.707106781186548));
#16843=DIRECTION('center_axis',(-1.,0.,0.));
#16844=DIRECTION('ref_axis',(0.,0.,-1.));
#16845=DIRECTION('center_axis',(1.,0.,0.));
#16846=DIRECTION('ref_axis',(0.,0.,-1.));
#16847=DIRECTION('',(0.,-1.,0.));
#16848=DIRECTION('center_axis',(-1.,0.,0.));
#16849=DIRECTION('ref_axis',(0.,1.,-6.12323399573677E-17));
#16850=DIRECTION('',(0.,1.,0.));
#16851=DIRECTION('center_axis',(-1.,0.,0.));
#16852=DIRECTION('ref_axis',(0.,0.,1.));
#16853=DIRECTION('',(0.,0.,-1.));
#16854=DIRECTION('center_axis',(-1.,0.,0.));
#16855=DIRECTION('ref_axis',(0.,0.,-1.));
#16856=DIRECTION('center_axis',(1.,0.,0.));
#16857=DIRECTION('ref_axis',(0.,0.,-1.));
#16858=DIRECTION('center_axis',(1.,0.,0.));
#16859=DIRECTION('ref_axis',(0.,0.,-1.));
#16860=DIRECTION('',(1.,0.,0.));
#16861=DIRECTION('center_axis',(0.,0.,1.));
#16862=DIRECTION('ref_axis',(1.,0.,0.));
#16863=DIRECTION('',(0.707106781186547,8.65956056235493E-17,-0.707106781186547));
#16864=DIRECTION('center_axis',(0.,0.,-1.));
#16865=DIRECTION('ref_axis',(1.,0.,0.));
#16866=DIRECTION('center_axis',(0.,0.,-1.));
#16867=DIRECTION('ref_axis',(1.,0.,0.));
#16868=DIRECTION('',(0.,0.,-1.));
#16869=DIRECTION('center_axis',(0.,0.,-1.));
#16870=DIRECTION('ref_axis',(1.,0.,0.));
#16871=DIRECTION('center_axis',(1.,0.,0.));
#16872=DIRECTION('ref_axis',(0.,0.,-1.));
#16873=DIRECTION('center_axis',(1.,0.,0.));
#16874=DIRECTION('ref_axis',(0.,0.,-1.));
#16875=DIRECTION('',(-0.707106781186554,8.65956056235486E-17,-0.707106781186541));
#16876=DIRECTION('center_axis',(-1.,0.,0.));
#16877=DIRECTION('ref_axis',(0.,0.,-1.));
#16878=DIRECTION('center_axis',(1.,0.,0.));
#16879=DIRECTION('ref_axis',(0.,0.,-1.));
#16880=DIRECTION('',(0.,-1.,0.));
#16881=DIRECTION('center_axis',(-1.,0.,0.));
#16882=DIRECTION('ref_axis',(0.,0.707106781186547,-0.707106781186547));
#16883=DIRECTION('',(0.,0.,-1.));
#16884=DIRECTION('center_axis',(-1.,0.,0.));
#16885=DIRECTION('ref_axis',(0.,0.707106781186547,0.707106781186547));
#16886=DIRECTION('',(0.,1.,0.));
#16887=DIRECTION('center_axis',(-1.,0.,0.));
#16888=DIRECTION('ref_axis',(0.,-0.707106781186547,0.707106781186547));
#16889=DIRECTION('',(0.,0.,1.));
#16890=DIRECTION('center_axis',(-1.,0.,0.));
#16891=DIRECTION('ref_axis',(0.,-0.707106781186547,-0.707106781186547));
#16892=DIRECTION('center_axis',(1.,0.,0.));
#16893=DIRECTION('ref_axis',(0.,0.,-1.));
#16894=DIRECTION('center_axis',(1.,0.,0.));
#16895=DIRECTION('ref_axis',(0.,0.,-1.));
#16896=DIRECTION('center_axis',(1.,0.,0.));
#16897=DIRECTION('ref_axis',(0.,1.,0.));
#16898=DIRECTION('center_axis',(1.,0.,0.));
#16899=DIRECTION('ref_axis',(0.,0.,-1.));
#16900=DIRECTION('center_axis',(-1.,0.,0.));
#16901=DIRECTION('ref_axis',(0.,0.,-1.));
#16902=DIRECTION('',(-1.,0.,0.));
#16903=DIRECTION('center_axis',(-1.,0.,0.));
#16904=DIRECTION('ref_axis',(0.,0.,-1.));
#16905=DIRECTION('center_axis',(1.,0.,0.));
#16906=DIRECTION('ref_axis',(0.,0.,-1.));
#16907=DIRECTION('',(-0.707106781186554,8.65956056235486E-17,-0.707106781186541));
#16908=DIRECTION('center_axis',(-1.,0.,0.));
#16909=DIRECTION('ref_axis',(0.,0.,-1.));
#16910=DIRECTION('center_axis',(-1.,0.,0.));
#16911=DIRECTION('ref_axis',(0.,0.,-1.));
#16912=DIRECTION('',(-1.,0.,0.));
#16913=DIRECTION('center_axis',(-1.,0.,0.));
#16914=DIRECTION('ref_axis',(0.,0.,-1.));
#16915=DIRECTION('center_axis',(1.,0.,0.));
#16916=DIRECTION('ref_axis',(0.,0.,-1.));
#16917=DIRECTION('',(-0.707106781186554,8.65956056235486E-17,-0.707106781186541));
#16918=DIRECTION('center_axis',(-1.,0.,0.));
#16919=DIRECTION('ref_axis',(0.,0.,-1.));
#16920=DIRECTION('center_axis',(-1.,0.,0.));
#16921=DIRECTION('ref_axis',(0.,0.,-1.));
#16922=DIRECTION('',(-1.,0.,0.));
#16923=DIRECTION('center_axis',(-1.,0.,0.));
#16924=DIRECTION('ref_axis',(0.,0.,-1.));
#16925=DIRECTION('center_axis',(1.,0.,0.));
#16926=DIRECTION('ref_axis',(0.,0.,-1.));
#16927=DIRECTION('',(-0.707106781186554,8.65956056235486E-17,-0.707106781186541));
#16928=DIRECTION('center_axis',(-1.,0.,0.));
#16929=DIRECTION('ref_axis',(0.,0.,-1.));
#16930=DIRECTION('center_axis',(-1.,0.,0.));
#16931=DIRECTION('ref_axis',(0.,0.,-1.));
#16932=DIRECTION('',(-1.,0.,0.));
#16933=DIRECTION('center_axis',(-1.,0.,0.));
#16934=DIRECTION('ref_axis',(0.,0.,-1.));
#16935=DIRECTION('center_axis',(-1.,0.,0.));
#16936=DIRECTION('ref_axis',(0.,0.,-1.));
#16937=DIRECTION('center_axis',(1.,0.,0.));
#16938=DIRECTION('ref_axis',(0.,0.,-1.));
#16939=DIRECTION('center_axis',(0.,-0.989664670474115,-0.143400976340336));
#16940=DIRECTION('ref_axis',(0.,0.143400976340336,-0.989664670474115));
#16941=DIRECTION('',(1.,0.,0.));
#16942=DIRECTION('center_axis',(0.,-0.989664670474115,-0.143400976340336));
#16943=DIRECTION('ref_axis',(0.,-0.143400976340336,0.989664670474115));
#16944=DIRECTION('',(-1.,0.,0.));
#16945=DIRECTION('center_axis',(0.,-1.,0.));
#16946=DIRECTION('ref_axis',(0.,0.,-1.));
#16947=DIRECTION('',(0.,0.,1.));
#16948=DIRECTION('',(1.,0.,0.));
#16949=DIRECTION('',(0.,0.,-1.));
#16950=DIRECTION('',(1.,0.,0.));
#16951=DIRECTION('',(0.,0.,1.));
#16952=DIRECTION('',(1.,0.,0.));
#16953=DIRECTION('center_axis',(0.,-0.143400976340336,-0.989664670474115));
#16954=DIRECTION('ref_axis',(-1.,0.,0.));
#16955=DIRECTION('',(1.,0.,0.));
#16956=DIRECTION('center_axis',(0.,-0.143400976340336,-0.989664670474115));
#16957=DIRECTION('ref_axis',(0.,0.989664670474115,-0.143400976340336));
#16958=DIRECTION('',(-1.,0.,0.));
#16959=DIRECTION('center_axis',(0.,0.,-1.));
#16960=DIRECTION('ref_axis',(0.,1.,0.));
#16961=DIRECTION('',(0.,-1.,0.));
#16962=DIRECTION('',(0.,-1.,0.));
#16963=DIRECTION('',(-1.,0.,0.));
#16964=DIRECTION('',(0.,-1.,0.));
#16965=DIRECTION('',(1.,0.,0.));
#16966=DIRECTION('',(1.,0.,0.));
#16967=DIRECTION('',(0.,1.,0.));
#16968=DIRECTION('',(1.,0.,0.));
#16969=DIRECTION('center_axis',(0.,0.143400976340336,-0.989664670474115));
#16970=DIRECTION('ref_axis',(-1.,0.,0.));
#16971=DIRECTION('center_axis',(0.,0.143400976340336,-0.989664670474115));
#16972=DIRECTION('ref_axis',(0.,-0.989664670474115,-0.143400976340336));
#16973=DIRECTION('',(1.,0.,0.));
#16974=DIRECTION('center_axis',(-1.,0.,0.));
#16975=DIRECTION('ref_axis',(0.,0.,-1.));
#16976=DIRECTION('center_axis',(1.,0.,0.));
#16977=DIRECTION('ref_axis',(0.,0.,-1.));
#16978=DIRECTION('center_axis',(0.,0.989664670474115,-0.143400976340336));
#16979=DIRECTION('ref_axis',(0.,0.143400976340336,0.989664670474115));
#16980=DIRECTION('',(1.,0.,0.));
#16981=DIRECTION('center_axis',(0.,0.989664670474115,-0.143400976340336));
#16982=DIRECTION('ref_axis',(0.,0.143400976340336,0.989664670474115));
#16983=DIRECTION('',(-1.,0.,0.));
#16984=DIRECTION('center_axis',(1.,0.,0.));
#16985=DIRECTION('ref_axis',(0.,0.,-1.));
#16986=DIRECTION('',(1.,0.,0.));
#16987=DIRECTION('center_axis',(-1.,0.,0.));
#16988=DIRECTION('ref_axis',(0.,-1.11022302462516E-16,-1.));
#16989=DIRECTION('',(1.,0.,0.));
#16990=DIRECTION('center_axis',(1.,0.,0.));
#16991=DIRECTION('ref_axis',(0.,0.,-1.));
#16992=DIRECTION('center_axis',(1.,0.,0.));
#16993=DIRECTION('ref_axis',(0.,0.,-1.));
#16994=DIRECTION('center_axis',(1.,0.,0.));
#16995=DIRECTION('ref_axis',(0.,0.,-1.));
#16996=DIRECTION('center_axis',(-1.,0.,0.));
#16997=DIRECTION('ref_axis',(0.,0.,1.));
#16998=DIRECTION('center_axis',(1.,0.,0.));
#16999=DIRECTION('ref_axis',(0.,0.,1.));
#17000=DIRECTION('center_axis',(0.,0.989664670474115,0.143400976340336));
#17001=DIRECTION('ref_axis',(0.,-0.143400976340336,0.989664670474115));
#17002=DIRECTION('',(1.,0.,0.));
#17003=DIRECTION('center_axis',(0.,0.989664670474115,0.143400976340336));
#17004=DIRECTION('ref_axis',(0.,0.143400976340336,-0.989664670474115));
#17005=DIRECTION('',(-1.,0.,0.));
#17006=DIRECTION('center_axis',(0.,1.,0.));
#17007=DIRECTION('ref_axis',(0.,0.,1.));
#17008=DIRECTION('',(0.,0.,-1.));
#17009=DIRECTION('',(1.,0.,0.));
#17010=DIRECTION('',(0.,0.,1.));
#17011=DIRECTION('',(1.,0.,0.));
#17012=DIRECTION('',(0.,0.,-1.));
#17013=DIRECTION('center_axis',(0.,0.143400976340336,0.989664670474115));
#17014=DIRECTION('ref_axis',(1.,0.,0.));
#17015=DIRECTION('',(1.,0.,0.));
#17016=DIRECTION('center_axis',(0.,0.143400976340336,0.989664670474115));
#17017=DIRECTION('ref_axis',(0.,-0.989664670474115,0.143400976340336));
#17018=DIRECTION('',(-1.,0.,0.));
#17019=DIRECTION('center_axis',(0.,0.,1.));
#17020=DIRECTION('ref_axis',(0.,-1.,0.));
#17021=DIRECTION('',(0.,1.,0.));
#17022=DIRECTION('',(0.,1.,0.));
#17023=DIRECTION('',(-1.,0.,0.));
#17024=DIRECTION('',(0.,1.,0.));
#17025=DIRECTION('',(1.,0.,0.));
#17026=DIRECTION('',(0.,-1.,0.));
#17027=DIRECTION('',(1.,0.,0.));
#17028=DIRECTION('',(1.,0.,0.));
#17029=DIRECTION('center_axis',(0.,-0.143400976340336,0.989664670474115));
#17030=DIRECTION('ref_axis',(1.,0.,0.));
#17031=DIRECTION('center_axis',(0.,-0.143400976340336,0.989664670474115));
#17032=DIRECTION('ref_axis',(0.,0.989664670474115,0.143400976340336));
#17033=DIRECTION('',(1.,0.,0.));
#17034=DIRECTION('center_axis',(-1.,0.,0.));
#17035=DIRECTION('ref_axis',(0.,0.,1.));
#17036=DIRECTION('center_axis',(1.,0.,0.));
#17037=DIRECTION('ref_axis',(0.,0.,1.));
#17038=DIRECTION('center_axis',(0.,-0.989664670474115,0.143400976340336));
#17039=DIRECTION('ref_axis',(0.,-0.143400976340336,-0.989664670474115));
#17040=DIRECTION('center_axis',(0.,-0.989664670474115,0.143400976340336));
#17041=DIRECTION('ref_axis',(0.,-0.143400976340336,-0.989664670474115));
#17042=DIRECTION('',(-1.,0.,0.));
#17043=DIRECTION('center_axis',(1.,0.,0.));
#17044=DIRECTION('ref_axis',(0.,1.22464679914735E-16,1.));
#17045=DIRECTION('',(1.,0.,0.));
#17046=DIRECTION('center_axis',(-1.,0.,0.));
#17047=DIRECTION('ref_axis',(0.,0.0163578624861081,0.999866201216386));
#17048=DIRECTION('',(1.,0.,0.));
#17049=DIRECTION('center_axis',(1.,0.,0.));
#17050=DIRECTION('ref_axis',(0.,0.,-1.));
#17051=DIRECTION('center_axis',(1.,0.,0.));
#17052=DIRECTION('ref_axis',(0.,1.22464679914735E-16,1.));
#17053=DIRECTION('center_axis',(1.,0.,0.));
#17054=DIRECTION('ref_axis',(0.,0.,-1.));
#17055=DIRECTION('center_axis',(-1.,0.,0.));
#17056=DIRECTION('ref_axis',(0.,0.,-1.));
#17057=DIRECTION('center_axis',(-1.,0.,0.));
#17058=DIRECTION('ref_axis',(0.,0.,-1.));
#17059=DIRECTION('',(0.707106781186547,-8.65956056235494E-17,-0.707106781186548));
#17060=DIRECTION('center_axis',(1.,0.,0.));
#17061=DIRECTION('ref_axis',(0.,0.,-1.));
#17062=DIRECTION('center_axis',(1.,0.,0.));
#17063=DIRECTION('ref_axis',(0.,-1.11022302462516E-16,-1.));
#17064=DIRECTION('',(0.,1.,0.));
#17065=DIRECTION('center_axis',(1.,0.,0.));
#17066=DIRECTION('ref_axis',(0.,-1.,1.83697019872103E-16));
#17067=DIRECTION('',(0.,-1.,0.));
#17068=DIRECTION('center_axis',(1.,0.,0.));
#17069=DIRECTION('ref_axis',(0.,0.0163578624861081,0.999866201216386));
#17070=DIRECTION('',(0.,-1.,0.));
#17071=DIRECTION('center_axis',(1.,0.,0.));
#17072=DIRECTION('ref_axis',(0.,1.,-6.12323399573677E-17));
#17073=DIRECTION('',(0.,1.,0.));
#17074=DIRECTION('center_axis',(-1.,0.,0.));
#17075=DIRECTION('ref_axis',(0.,0.,-1.));
#17076=DIRECTION('center_axis',(1.,0.,0.));
#17077=DIRECTION('ref_axis',(0.,1.,0.));
#17078=DIRECTION('center_axis',(-1.,0.,0.));
#17079=DIRECTION('ref_axis',(0.,0.,-1.));
#17080=DIRECTION('',(0.707106781186547,-8.65956056235494E-17,-0.707106781186548));
#17081=DIRECTION('center_axis',(1.,0.,0.));
#17082=DIRECTION('ref_axis',(0.,-1.22464679914735E-16,1.));
#17083=DIRECTION('center_axis',(0.,-1.,0.));
#17084=DIRECTION('ref_axis',(-0.707106781186548,0.,0.707106781186547));
#17085=DIRECTION('center_axis',(0.,1.,-4.44089209850063E-15));
#17086=DIRECTION('ref_axis',(-1.,0.,0.));
#17087=DIRECTION('',(0.,1.,0.));
#17088=DIRECTION('center_axis',(1.,0.,0.));
#17089=DIRECTION('ref_axis',(0.,0.,-1.));
#17090=DIRECTION('center_axis',(0.,-1.,0.));
#17091=DIRECTION('ref_axis',(-1.,0.,0.));
#17092=DIRECTION('center_axis',(-1.,0.,0.));
#17093=DIRECTION('ref_axis',(0.,-1.,1.83697019872103E-16));
#17094=DIRECTION('center_axis',(0.,1.,0.));
#17095=DIRECTION('ref_axis',(-0.707106781186548,0.,-0.707106781186547));
#17096=DIRECTION('',(0.,-1.,0.));
#17097=DIRECTION('center_axis',(1.,0.,0.));
#17098=DIRECTION('ref_axis',(0.,0.,-1.));
#17099=DIRECTION('center_axis',(1.,0.,0.));
#17100=DIRECTION('ref_axis',(0.,0.,-1.));
#17101=DIRECTION('center_axis',(0.,1.,0.));
#17102=DIRECTION('ref_axis',(0.,0.,-1.));
#17103=DIRECTION('center_axis',(0.,1.,0.));
#17104=DIRECTION('ref_axis',(-1.,0.,0.));
#17105=DIRECTION('center_axis',(-1.,0.,0.));
#17106=DIRECTION('ref_axis',(0.,1.,-6.12323399573677E-17));
#17107=DIRECTION('center_axis',(0.,-1.,0.));
#17108=DIRECTION('ref_axis',(-0.707106781186548,0.,0.707106781186547));
#17109=DIRECTION('',(0.,1.,0.));
#17110=DIRECTION('center_axis',(0.,1.,0.));
#17111=DIRECTION('ref_axis',(-0.707106781186548,0.,-0.707106781186547));
#17112=DIRECTION('',(0.,-1.,0.));
#17113=DIRECTION('center_axis',(1.,0.,0.));
#17114=DIRECTION('ref_axis',(0.,0.,-1.));
#17115=DIRECTION('',(1.,0.,0.));
#17116=DIRECTION('center_axis',(1.,0.,0.));
#17117=DIRECTION('ref_axis',(0.,1.,-6.12323399573677E-17));
#17118=DIRECTION('',(1.,0.,0.));
#17119=DIRECTION('center_axis',(0.,0.,1.));
#17120=DIRECTION('ref_axis',(0.,-1.,0.));
#17121=DIRECTION('',(0.,-1.,0.));
#17122=DIRECTION('center_axis',(1.,0.,0.));
#17123=DIRECTION('ref_axis',(0.,1.22464679914735E-16,1.));
#17124=DIRECTION('center_axis',(-1.,0.,0.));
#17125=DIRECTION('ref_axis',(0.,1.22464679914735E-16,1.));
#17126=DIRECTION('center_axis',(0.,-1.,0.));
#17127=DIRECTION('ref_axis',(0.707106781186548,0.,0.707106781186548));
#17128=DIRECTION('center_axis',(0.,1.,-4.44089209850063E-15));
#17129=DIRECTION('ref_axis',(0.,4.44089209850063E-15,1.));
#17130=DIRECTION('',(0.,-1.,0.));
#17131=DIRECTION('center_axis',(1.,0.,0.));
#17132=DIRECTION('ref_axis',(0.,0.,-1.));
#17133=DIRECTION('center_axis',(0.,-1.,0.));
#17134=DIRECTION('ref_axis',(0.,0.,-1.));
#17135=DIRECTION('center_axis',(1.,0.,0.));
#17136=DIRECTION('ref_axis',(0.,-1.,1.83697019872103E-16));
#17137=DIRECTION('center_axis',(0.,1.,0.));
#17138=DIRECTION('ref_axis',(0.707106781186548,0.,-0.707106781186548));
#17139=DIRECTION('',(0.,1.,0.));
#17140=DIRECTION('center_axis',(0.,0.,-1.));
#17141=DIRECTION('ref_axis',(0.,1.,0.));
#17142=DIRECTION('',(1.,0.,0.));
#17143=DIRECTION('center_axis',(1.,0.,0.));
#17144=DIRECTION('ref_axis',(0.,0.,-1.));
#17145=DIRECTION('',(1.,0.,0.));
#17146=DIRECTION('center_axis',(0.,0.,1.));
#17147=DIRECTION('ref_axis',(0.,-1.,0.));
#17148=DIRECTION('center_axis',(1.,0.,0.));
#17149=DIRECTION('ref_axis',(0.,0.,-1.));
#17150=DIRECTION('center_axis',(-1.,0.,0.));
#17151=DIRECTION('ref_axis',(0.,0.,-1.));
#17152=DIRECTION('center_axis',(0.,1.,0.));
#17153=DIRECTION('ref_axis',(0.707106781186548,0.,-0.707106781186548));
#17154=DIRECTION('center_axis',(0.,-1.,4.44089209850063E-15));
#17155=DIRECTION('ref_axis',(0.,-4.44089209850063E-15,-1.));
#17156=DIRECTION('',(0.,1.,0.));
#17157=DIRECTION('center_axis',(1.,0.,0.));
#17158=DIRECTION('ref_axis',(0.,0.,-1.));
#17159=DIRECTION('center_axis',(0.,1.,0.));
#17160=DIRECTION('ref_axis',(0.,0.,1.));
#17161=DIRECTION('center_axis',(0.,-1.,0.));
#17162=DIRECTION('ref_axis',(0.707106781186548,0.,0.707106781186548));
#17163=DIRECTION('center_axis',(0.,0.,-1.));
#17164=DIRECTION('ref_axis',(0.,1.,0.));
#17165=DIRECTION('center_axis',(1.,0.,0.));
#17166=DIRECTION('ref_axis',(0.,1.,-1.84400444715477E-16));
#17167=DIRECTION('center_axis',(-1.,0.,0.));
#17168=DIRECTION('ref_axis',(0.,1.,-1.84400444715477E-16));
#17169=DIRECTION('center_axis',(0.,-3.06865124630212E-16,-1.));
#17170=DIRECTION('ref_axis',(0.,-1.,3.06865124630213E-16));
#17171=DIRECTION('center_axis',(1.,0.,0.));
#17172=DIRECTION('ref_axis',(0.,0.,-1.));
#17173=DIRECTION('center_axis',(1.,0.,0.));
#17174=DIRECTION('ref_axis',(0.,1.,0.));
#17175=DIRECTION('',(-1.,0.,0.));
#17176=DIRECTION('center_axis',(0.,-1.,0.));
#17177=DIRECTION('ref_axis',(-0.707106781186545,0.,0.70710678118655));
#17178=DIRECTION('',(0.,-1.,0.));
#17179=DIRECTION('center_axis',(0.,1.,-2.22044604925031E-15));
#17180=DIRECTION('ref_axis',(-1.,0.,0.));
#17181=DIRECTION('center_axis',(1.,0.,0.));
#17182=DIRECTION('ref_axis',(0.,0.,-1.));
#17183=DIRECTION('center_axis',(0.,0.,1.));
#17184=DIRECTION('ref_axis',(-1.,0.,0.));
#17185=DIRECTION('center_axis',(-1.,0.,0.));
#17186=DIRECTION('ref_axis',(0.,-0.707106781186548,0.707106781186548));
#17187=DIRECTION('center_axis',(1.,0.,0.));
#17188=DIRECTION('ref_axis',(0.,-0.707106781186547,0.707106781186547));
#17189=DIRECTION('center_axis',(0.,0.,-1.));
#17190=DIRECTION('ref_axis',(-0.707106781186545,-0.70710678118655,0.));
#17191=DIRECTION('',(0.,0.,-1.));
#17192=DIRECTION('center_axis',(1.,0.,0.));
#17193=DIRECTION('ref_axis',(0.,0.,-1.));
#17194=DIRECTION('center_axis',(1.,0.,0.));
#17195=DIRECTION('ref_axis',(0.,0.,-1.));
#17196=DIRECTION('center_axis',(0.,0.,1.));
#17197=DIRECTION('ref_axis',(0.,1.,0.));
#17198=DIRECTION('center_axis',(1.,0.,0.));
#17199=DIRECTION('ref_axis',(0.,0.707106781186547,0.707106781186547));
#17200=DIRECTION('center_axis',(0.,1.,0.));
#17201=DIRECTION('ref_axis',(-1.,0.,0.));
#17202=DIRECTION('center_axis',(-1.,0.,0.));
#17203=DIRECTION('ref_axis',(0.,0.707106781186548,0.707106781186548));
#17204=DIRECTION('center_axis',(0.,-1.,0.));
#17205=DIRECTION('ref_axis',(-0.707106781186545,0.,0.70710678118655));
#17206=DIRECTION('',(0.,-1.,0.));
#17207=DIRECTION('center_axis',(0.,0.,1.));
#17208=DIRECTION('ref_axis',(-0.707106781186545,0.70710678118655,0.));
#17209=DIRECTION('',(0.,0.,1.));
#17210=DIRECTION('center_axis',(1.,0.,0.));
#17211=DIRECTION('ref_axis',(0.,0.,-1.));
#17212=DIRECTION('center_axis',(0.,1.,0.));
#17213=DIRECTION('ref_axis',(-0.707106781186545,0.,-0.70710678118655));
#17214=DIRECTION('',(0.,1.,0.));
#17215=DIRECTION('center_axis',(0.,-1.,2.22044604925031E-15));
#17216=DIRECTION('ref_axis',(-1.,0.,0.));
#17217=DIRECTION('center_axis',(1.,0.,0.));
#17218=DIRECTION('ref_axis',(0.,0.,-1.));
#17219=DIRECTION('center_axis',(0.,0.,-1.));
#17220=DIRECTION('ref_axis',(-1.,0.,0.));
#17221=DIRECTION('center_axis',(-1.,0.,0.));
#17222=DIRECTION('ref_axis',(0.,0.707106781186548,-0.707106781186548));
#17223=DIRECTION('center_axis',(1.,0.,0.));
#17224=DIRECTION('ref_axis',(0.,0.707106781186547,-0.707106781186547));
#17225=DIRECTION('center_axis',(0.,0.,1.));
#17226=DIRECTION('ref_axis',(-0.707106781186545,0.70710678118655,0.));
#17227=DIRECTION('',(0.,0.,1.));
#17228=DIRECTION('center_axis',(1.,0.,0.));
#17229=DIRECTION('ref_axis',(0.,0.,-1.));
#17230=DIRECTION('center_axis',(0.,0.,-1.));
#17231=DIRECTION('ref_axis',(-0.707106781186545,-0.70710678118655,0.));
#17232=DIRECTION('',(0.,0.,-1.));
#17233=DIRECTION('center_axis',(0.,2.22044604925031E-15,1.));
#17234=DIRECTION('ref_axis',(-1.,0.,0.));
#17235=DIRECTION('center_axis',(1.,0.,0.));
#17236=DIRECTION('ref_axis',(0.,0.,-1.));
#17237=DIRECTION('center_axis',(0.,-1.,0.));
#17238=DIRECTION('ref_axis',(-1.,0.,0.));
#17239=DIRECTION('center_axis',(-1.,0.,0.));
#17240=DIRECTION('ref_axis',(0.,-0.707106781186548,-0.707106781186548));
#17241=DIRECTION('center_axis',(1.,0.,0.));
#17242=DIRECTION('ref_axis',(0.,-0.707106781186547,-0.707106781186547));
#17243=DIRECTION('center_axis',(0.,1.,0.));
#17244=DIRECTION('ref_axis',(-0.707106781186545,0.,-0.70710678118655));
#17245=DIRECTION('',(0.,1.,0.));
#17246=DIRECTION('center_axis',(1.,0.,0.));
#17247=DIRECTION('ref_axis',(0.,0.,-1.));
#17248=DIRECTION('center_axis',(0.,1.,0.));
#17249=DIRECTION('ref_axis',(0.707106781186544,0.,-0.707106781186551));
#17250=DIRECTION('center_axis',(0.,1.,0.));
#17251=DIRECTION('ref_axis',(1.,0.,0.));
#17252=DIRECTION('center_axis',(0.,-1.,2.22044604925031E-15));
#17253=DIRECTION('ref_axis',(0.,-2.22044604925031E-15,-1.));
#17254=DIRECTION('center_axis',(1.,0.,0.));
#17255=DIRECTION('ref_axis',(0.,0.,-1.));
#17256=DIRECTION('center_axis',(0.,0.,-1.));
#17257=DIRECTION('ref_axis',(0.,1.,0.));
#17258=DIRECTION('center_axis',(1.,0.,0.));
#17259=DIRECTION('ref_axis',(0.,0.707106781186548,-0.707106781186548));
#17260=DIRECTION('center_axis',(0.,0.,1.));
#17261=DIRECTION('ref_axis',(0.707106781186544,0.707106781186551,0.));
#17262=DIRECTION('center_axis',(0.,-2.22044604925031E-15,-1.));
#17263=DIRECTION('ref_axis',(0.,1.,-2.22044604925031E-15));
#17264=DIRECTION('center_axis',(1.,0.,0.));
#17265=DIRECTION('ref_axis',(0.,0.,-1.));
#17266=DIRECTION('center_axis',(0.,1.,0.));
#17267=DIRECTION('ref_axis',(0.,0.,1.));
#17268=DIRECTION('center_axis',(1.,0.,0.));
#17269=DIRECTION('ref_axis',(0.,0.707106781186548,0.707106781186548));
#17270=DIRECTION('center_axis',(0.,-1.,0.));
#17271=DIRECTION('ref_axis',(0.707106781186544,0.,0.707106781186551));
#17272=DIRECTION('center_axis',(0.,1.,-2.22044604925031E-15));
#17273=DIRECTION('ref_axis',(0.,2.22044604925031E-15,1.));
#17274=DIRECTION('center_axis',(1.,0.,0.));
#17275=DIRECTION('ref_axis',(0.,0.,-1.));
#17276=DIRECTION('center_axis',(0.,0.,1.));
#17277=DIRECTION('ref_axis',(0.,-1.,0.));
#17278=DIRECTION('center_axis',(1.,0.,0.));
#17279=DIRECTION('ref_axis',(0.,-0.707106781186548,0.707106781186548));
#17280=DIRECTION('center_axis',(0.,0.,-1.));
#17281=DIRECTION('ref_axis',(0.707106781186544,-0.707106781186551,0.));
#17282=DIRECTION('center_axis',(0.,2.22044604925031E-15,1.));
#17283=DIRECTION('ref_axis',(0.,-1.,2.22044604925031E-15));
#17284=DIRECTION('center_axis',(1.,0.,0.));
#17285=DIRECTION('ref_axis',(0.,0.,-1.));
#17286=DIRECTION('center_axis',(1.,0.,0.));
#17287=DIRECTION('ref_axis',(0.,-0.707106781186548,-0.707106781186548));
#17288=DIRECTION('center_axis',(1.,0.,0.));
#17289=DIRECTION('ref_axis',(0.,1.,1.58603289232165E-16));
#17290=DIRECTION('center_axis',(1.,0.,0.));
#17291=DIRECTION('ref_axis',(0.,1.58603289232165E-16,-1.));
#17292=DIRECTION('center_axis',(-1.,0.,0.));
#17293=DIRECTION('ref_axis',(0.,0.,1.));
#17294=DIRECTION('center_axis',(0.,-1.,1.22464679914735E-16));
#17295=DIRECTION('ref_axis',(0.,-1.22464679914735E-16,-1.));
#17296=DIRECTION('center_axis',(-1.,0.,0.));
#17297=DIRECTION('ref_axis',(0.,1.,0.));
#17298=DIRECTION('center_axis',(-1.,0.,0.));
#17299=DIRECTION('ref_axis',(0.,1.,0.));
#17300=DIRECTION('center_axis',(1.,0.,0.));
#17301=DIRECTION('ref_axis',(0.,1.,0.));
#17302=DIRECTION('center_axis',(1.,0.,0.));
#17303=DIRECTION('ref_axis',(0.,0.,-1.));
#17304=DIRECTION('',(1.,0.,0.));
#17305=DIRECTION('center_axis',(-0.518601214467743,-0.756360525034703,0.39871234809297));
#17306=DIRECTION('ref_axis',(0.,-0.466321371218455,-0.884615384641789));
#17307=DIRECTION('center_axis',(-0.518601214553226,0.756360524966231,-0.398712348111676));
#17308=DIRECTION('ref_axis',(0.,-0.466321371268611,-0.884615384615349));
#17309=DIRECTION('center_axis',(0.518601214467742,-0.756360525034697,-0.398712348092983));
#17310=DIRECTION('ref_axis',(4.44089209850065E-15,-0.466321371218468,0.884615384641782));
#17311=DIRECTION('center_axis',(0.518601214552952,0.756360524966382,0.398712348111745));
#17312=DIRECTION('ref_axis',(0.,-0.466321371268601,0.884615384615355));
#17313=DIRECTION('center_axis',(0.,0.,1.));
#17314=DIRECTION('ref_axis',(1.,0.,0.));
#17315=DIRECTION('center_axis',(0.,0.,1.));
#17316=DIRECTION('ref_axis',(1.,0.,0.));
#17317=DIRECTION('',(0.,0.,1.));
#17318=DIRECTION('center_axis',(1.,0.,0.));
#17319=DIRECTION('ref_axis',(0.,0.,-1.));
#17320=DIRECTION('center_axis',(1.,0.,0.));
#17321=DIRECTION('ref_axis',(0.,0.,-1.));
#17322=DIRECTION('center_axis',(1.,0.,0.));
#17323=DIRECTION('ref_axis',(0.,0.,-1.));
#17324=DIRECTION('center_axis',(1.,0.,0.));
#17325=DIRECTION('ref_axis',(0.,0.,-1.));
#17326=DIRECTION('center_axis',(1.,0.,0.));
#17327=DIRECTION('ref_axis',(0.,1.,0.));
#17328=DIRECTION('center_axis',(1.,0.,0.));
#17329=DIRECTION('ref_axis',(0.,1.,0.));
#17330=DIRECTION('',(1.,0.,0.));
#17331=DIRECTION('center_axis',(1.,0.,0.));
#17332=DIRECTION('ref_axis',(0.,0.,-1.));
#17333=DIRECTION('center_axis',(-1.,0.,0.));
#17334=DIRECTION('ref_axis',(0.,0.,1.));
#17335=DIRECTION('center_axis',(1.,0.,0.));
#17336=DIRECTION('ref_axis',(0.,0.,-1.));
#17337=DIRECTION('center_axis',(1.,0.,0.));
#17338=DIRECTION('ref_axis',(0.,1.,0.));
#17339=DIRECTION('',(1.,0.,0.));
#17340=DIRECTION('center_axis',(1.,0.,0.));
#17341=DIRECTION('ref_axis',(0.,0.,-1.));
#17342=DIRECTION('center_axis',(1.,0.,0.));
#17343=DIRECTION('ref_axis',(0.,0.,-1.));
#17344=DIRECTION('center_axis',(1.,0.,0.));
#17345=DIRECTION('ref_axis',(0.,0.,-1.));
#17346=DIRECTION('center_axis',(1.,0.,0.));
#17347=DIRECTION('ref_axis',(0.,1.,0.));
#17348=DIRECTION('',(1.,0.,0.));
#17349=DIRECTION('center_axis',(1.,0.,0.));
#17350=DIRECTION('ref_axis',(0.,0.,-1.));
#17351=DIRECTION('center_axis',(-1.,0.,0.));
#17352=DIRECTION('ref_axis',(0.,0.,1.));
#17353=DIRECTION('center_axis',(-1.,0.,0.));
#17354=DIRECTION('ref_axis',(0.,0.,1.));
#17355=DIRECTION('center_axis',(1.,0.,0.));
#17356=DIRECTION('ref_axis',(0.,-1.58603289232165E-16,1.));
#17357=DIRECTION('center_axis',(1.,0.,0.));
#17358=DIRECTION('ref_axis',(0.,-1.,-1.58603289232165E-16));
#17359=DIRECTION('center_axis',(1.,0.,0.));
#17360=DIRECTION('ref_axis',(0.,0.,-1.));
#17361=DIRECTION('center_axis',(1.,0.,0.));
#17362=DIRECTION('ref_axis',(0.,0.,-1.));
#17363=DIRECTION('axis',(0.,0.,1.));
#17364=DIRECTION('refdir',(1.,0.,0.));
#17365=DIRECTION('center_axis',(-1.,0.,0.));
#17366=DIRECTION('ref_axis',(0.,-1.,0.));
#17367=DIRECTION('center_axis',(-1.,0.,0.));
#17368=DIRECTION('ref_axis',(0.,-1.,0.));
#17369=DIRECTION('',(0.707106781186552,-0.707106781186543,8.65956056235488E-17));
#17370=DIRECTION('center_axis',(1.,0.,0.));
#17371=DIRECTION('ref_axis',(0.,-1.,0.));
#17372=DIRECTION('center_axis',(1.,0.,0.));
#17373=DIRECTION('ref_axis',(0.,-1.,0.));
#17374=DIRECTION('center_axis',(1.,0.,0.));
#17375=DIRECTION('ref_axis',(0.,0.,-1.));
#17376=DIRECTION('center_axis',(1.,0.,0.));
#17377=DIRECTION('ref_axis',(0.,0.,-1.));
#17378=DIRECTION('center_axis',(1.,0.,0.));
#17379=DIRECTION('ref_axis',(0.,1.,0.));
#17380=DIRECTION('',(1.,0.,0.));
#17381=DIRECTION('center_axis',(1.,0.,0.));
#17382=DIRECTION('ref_axis',(0.,0.,-1.));
#17383=DIRECTION('center_axis',(0.,-1.,0.));
#17384=DIRECTION('ref_axis',(1.,0.,0.));
#17385=DIRECTION('center_axis',(0.,-1.,0.));
#17386=DIRECTION('ref_axis',(1.,0.,0.));
#17387=DIRECTION('',(0.707106781186554,0.707106781186541,8.65956056235501E-17));
#17388=DIRECTION('center_axis',(0.,1.,0.));
#17389=DIRECTION('ref_axis',(1.,0.,0.));
#17390=DIRECTION('center_axis',(0.,-1.,0.));
#17391=DIRECTION('ref_axis',(1.,0.,0.));
#17392=DIRECTION('center_axis',(0.,-1.,0.));
#17393=DIRECTION('ref_axis',(-1.,0.,0.));
#17394=DIRECTION('',(1.,0.,0.));
#17395=DIRECTION('center_axis',(0.,-1.,0.));
#17396=DIRECTION('ref_axis',(1.,0.,0.));
#17397=DIRECTION('',(0.,0.,1.));
#17398=DIRECTION('center_axis',(0.,-1.,0.));
#17399=DIRECTION('ref_axis',(1.,0.,0.));
#17400=DIRECTION('',(-1.,0.,0.));
#17401=DIRECTION('center_axis',(0.,-1.,0.));
#17402=DIRECTION('ref_axis',(-1.,0.,0.));
#17403=DIRECTION('',(0.,0.,-1.));
#17404=DIRECTION('center_axis',(0.,1.,0.));
#17405=DIRECTION('ref_axis',(1.,0.,0.));
#17406=DIRECTION('',(0.,1.,0.));
#17407=DIRECTION('center_axis',(0.,1.,0.));
#17408=DIRECTION('ref_axis',(1.,0.,0.));
#17409=DIRECTION('center_axis',(0.,-1.,0.));
#17410=DIRECTION('ref_axis',(-1.,0.,0.));
#17411=DIRECTION('',(-0.555969453910032,0.707106781186556,0.436918718206223));
#17412=DIRECTION('center_axis',(0.,1.,0.));
#17413=DIRECTION('ref_axis',(-1.,0.,0.));
#17414=DIRECTION('center_axis',(0.,1.,0.));
#17415=DIRECTION('ref_axis',(-1.,0.,0.));
#17416=DIRECTION('',(-0.450316983320678,-0.707106781186556,0.545173930533139));
#17417=DIRECTION('',(0.406052535411294,-0.675506402763447,0.615477406824692));
#17418=DIRECTION('',(0.406052535411299,0.675506402763456,-0.615477406824679));
#17419=DIRECTION('center_axis',(0.,-1.,0.));
#17420=DIRECTION('ref_axis',(1.,0.,0.));
#17421=DIRECTION('',(-0.450316983320678,0.707106781186556,-0.545173930533139));
#17422=DIRECTION('center_axis',(0.,1.,0.));
#17423=DIRECTION('ref_axis',(1.,0.,0.));
#17424=DIRECTION('',(0.555969453910031,-0.707106781186554,0.436918718206228));
#17425=DIRECTION('center_axis',(0.,-1.,0.));
#17426=DIRECTION('ref_axis',(1.,0.,0.));
#17427=DIRECTION('',(0.628668104787158,-0.674217950114304,-0.387564923292846));
#17428=DIRECTION('',(-0.628668104787152,0.674217950114311,-0.387564923292843));
#17429=DIRECTION('center_axis',(0.,-1.,0.));
#17430=DIRECTION('ref_axis',(1.,0.,0.));
#17431=DIRECTION('',(0.,0.,-1.));
#17432=DIRECTION('',(1.,0.,0.));
#17433=DIRECTION('center_axis',(0.,0.,1.));
#17434=DIRECTION('ref_axis',(0.707106781186538,-0.707106781186557,0.));
#17435=DIRECTION('',(0.,0.,-1.));
#17436=DIRECTION('center_axis',(0.,0.,-1.));
#17437=DIRECTION('ref_axis',(0.707106781186543,-0.707106781186552,0.));
#17438=DIRECTION('',(0.,0.,1.));
#17439=DIRECTION('center_axis',(0.,0.,1.));
#17440=DIRECTION('ref_axis',(0.707106781186543,-0.707106781186552,0.));
#17441=DIRECTION('center_axis',(0.,1.,0.));
#17442=DIRECTION('ref_axis',(1.,0.,0.));
#17443=DIRECTION('',(0.,1.,0.));
#17444=DIRECTION('center_axis',(0.,1.,0.));
#17445=DIRECTION('ref_axis',(1.,0.,0.));
#17446=DIRECTION('center_axis',(0.,-1.,0.));
#17447=DIRECTION('ref_axis',(1.,0.,0.));
#17448=DIRECTION('',(-0.450316983320678,0.707106781186556,-0.545173930533139));
#17449=DIRECTION('center_axis',(0.,1.,0.));
#17450=DIRECTION('ref_axis',(1.,0.,0.));
#17451=DIRECTION('',(-0.469605266894875,-0.707106781186553,-0.528650066967352));
#17452=DIRECTION('',(-0.52464839659846,-0.683785150909193,0.507131075110525));
#17453=DIRECTION('',(0.524648396598484,0.683785150909177,0.507131075110523));
#17454=DIRECTION('center_axis',(0.,-1.,0.));
#17455=DIRECTION('ref_axis',(-1.,0.,0.));
#17456=DIRECTION('',(0.469605266894875,0.707106781186553,-0.528650066967352));
#17457=DIRECTION('center_axis',(0.,1.,0.));
#17458=DIRECTION('ref_axis',(-1.,0.,0.));
#17459=DIRECTION('',(-0.450316983320678,-0.707106781186556,0.545173930533139));
#17460=DIRECTION('center_axis',(0.,-1.,0.));
#17461=DIRECTION('ref_axis',(-1.,0.,0.));
#17462=DIRECTION('',(0.406052535411297,-0.675506402763453,0.615477406824684));
#17463=DIRECTION('',(0.406052535411268,0.675506402763462,-0.615477406824693));
#17464=DIRECTION('center_axis',(0.,-1.,0.));
#17465=DIRECTION('ref_axis',(1.,0.,0.));
#17466=DIRECTION('',(1.,0.,0.));
#17467=DIRECTION('',(0.,0.,1.));
#17468=DIRECTION('center_axis',(1.,0.,0.));
#17469=DIRECTION('ref_axis',(0.,-0.707106781186549,0.707106781186546));
#17470=DIRECTION('center_axis',(-1.,0.,0.));
#17471=DIRECTION('ref_axis',(0.,-1.,0.));
#17472=DIRECTION('',(-1.,0.,0.));
#17473=DIRECTION('center_axis',(-1.,0.,0.));
#17474=DIRECTION('ref_axis',(0.,0.,1.));
#17475=DIRECTION('center_axis',(0.,1.,0.));
#17476=DIRECTION('ref_axis',(1.,0.,0.));
#17477=DIRECTION('',(0.,1.,0.));
#17478=DIRECTION('center_axis',(0.,1.,0.));
#17479=DIRECTION('ref_axis',(1.,0.,0.));
#17480=DIRECTION('center_axis',(0.,-1.,0.));
#17481=DIRECTION('ref_axis',(1.,0.,0.));
#17482=DIRECTION('',(-0.555969453910031,0.707106781186554,0.436918718206228));
#17483=DIRECTION('center_axis',(0.,1.,0.));
#17484=DIRECTION('ref_axis',(1.,0.,0.));
#17485=DIRECTION('',(0.450316983320677,-0.707106781186554,-0.545173930533143));
#17486=DIRECTION('center_axis',(0.,-1.,0.));
#17487=DIRECTION('ref_axis',(1.,0.,0.));
#17488=DIRECTION('',(-0.406052535411294,-0.675506402763435,-0.615477406824705));
#17489=DIRECTION('',(-0.406052535411254,0.675506402763442,0.615477406824724));
#17490=DIRECTION('center_axis',(0.,-1.,0.));
#17491=DIRECTION('ref_axis',(-1.,0.,0.));
#17492=DIRECTION('',(0.450316983320678,0.707106781186556,0.545173930533139));
#17493=DIRECTION('center_axis',(0.,1.,0.));
#17494=DIRECTION('ref_axis',(-1.,0.,0.));
#17495=DIRECTION('center_axis',(0.,1.,0.));
#17496=DIRECTION('ref_axis',(-1.,0.,0.));
#17497=DIRECTION('',(0.555969453910031,-0.707106781186554,0.436918718206228));
#17498=DIRECTION('',(0.628668104787149,-0.674217950114307,-0.387564923292854));
#17499=DIRECTION('',(-0.628668104787158,0.674217950114304,-0.387564923292846));
#17500=DIRECTION('center_axis',(0.,1.,0.));
#17501=DIRECTION('ref_axis',(1.,0.,0.));
#17502=DIRECTION('',(0.,1.,0.));
#17503=DIRECTION('center_axis',(0.,1.,0.));
#17504=DIRECTION('ref_axis',(1.,0.,0.));
#17505=DIRECTION('center_axis',(0.,-1.,0.));
#17506=DIRECTION('ref_axis',(1.,0.,0.));
#17507=DIRECTION('',(0.469605266894875,0.707106781186553,-0.528650066967352));
#17508=DIRECTION('center_axis',(0.,1.,0.));
#17509=DIRECTION('ref_axis',(1.,0.,0.));
#17510=DIRECTION('',(0.450316983320697,-0.707106781186546,-0.545173930533137));
#17511=DIRECTION('',(-0.406052535411294,-0.675506402763447,-0.615477406824692));
#17512=DIRECTION('',(-0.406052535411272,0.675506402763455,0.615477406824698));
#17513=DIRECTION('center_axis',(0.,-1.,0.));
#17514=DIRECTION('ref_axis',(-1.,0.,0.));
#17515=DIRECTION('',(0.450316983320697,0.707106781186546,0.545173930533137));
#17516=DIRECTION('center_axis',(0.,1.,0.));
#17517=DIRECTION('ref_axis',(-1.,0.,0.));
#17518=DIRECTION('',(-0.469605266894875,-0.707106781186553,-0.528650066967352));
#17519=DIRECTION('center_axis',(0.,-1.,0.));
#17520=DIRECTION('ref_axis',(-1.,0.,0.));
#17521=DIRECTION('',(-0.524648396598479,-0.683785150909184,0.507131075110518));
#17522=DIRECTION('',(0.524648396598465,0.683785150909186,0.50713107511053));
#17523=DIRECTION('center_axis',(0.,-1.,0.));
#17524=DIRECTION('ref_axis',(1.,0.,0.));
#17525=DIRECTION('',(0.,0.,1.));
#17526=DIRECTION('',(-1.,0.,0.));
#17527=DIRECTION('center_axis',(0.,0.,1.));
#17528=DIRECTION('ref_axis',(-0.707106781186544,-0.707106781186551,0.));
#17529=DIRECTION('center_axis',(0.,0.,1.));
#17530=DIRECTION('ref_axis',(0.,-1.,0.));
#17531=DIRECTION('',(0.,0.,-1.));
#17532=DIRECTION('center_axis',(0.,0.,-1.));
#17533=DIRECTION('ref_axis',(-1.,0.,0.));
#17534=DIRECTION('center_axis',(0.,1.,0.));
#17535=DIRECTION('ref_axis',(1.,0.,0.));
#17536=DIRECTION('',(0.,1.,0.));
#17537=DIRECTION('center_axis',(0.,1.,0.));
#17538=DIRECTION('ref_axis',(1.,0.,0.));
#17539=DIRECTION('',(-0.706933664902991,-0.171973946473105,-0.686053755300042));
#17540=DIRECTION('center_axis',(-1.,0.,0.));
#17541=DIRECTION('ref_axis',(0.,-0.946352857512202,0.323135063214268));
#17542=DIRECTION('center_axis',(1.,0.,0.));
#17543=DIRECTION('ref_axis',(0.,-0.946352857512203,0.323135063214268));
#17544=DIRECTION('',(0.707106781186544,0.186221003615294,0.682144953666387));
#17545=DIRECTION('center_axis',(-1.,0.,0.));
#17546=DIRECTION('ref_axis',(0.,-0.946352857512202,0.323135063214268));
#17547=DIRECTION('center_axis',(-1.,0.,0.));
#17548=DIRECTION('ref_axis',(0.,0.946352857512202,-0.323135063214268));
#17549=DIRECTION('',(-1.,0.,0.));
#17550=DIRECTION('center_axis',(-1.,0.,0.));
#17551=DIRECTION('ref_axis',(0.,0.946352857512202,-0.323135063214268));
#17552=DIRECTION('',(1.,0.,0.));
#17553=DIRECTION('',(0.706933664902985,0.171973946473104,-0.686053755300049));
#17554=DIRECTION('center_axis',(-1.,0.,0.));
#17555=DIRECTION('ref_axis',(0.,-0.946352857512202,-0.323135063214268));
#17556=DIRECTION('',(-0.707106781186544,-0.186221003615294,0.682144953666387));
#17557=DIRECTION('center_axis',(1.,0.,0.));
#17558=DIRECTION('ref_axis',(0.,-0.946352857512203,-0.323135063214268));
#17559=DIRECTION('center_axis',(-1.,0.,0.));
#17560=DIRECTION('ref_axis',(0.,-0.946352857512202,-0.323135063214268));
#17561=DIRECTION('center_axis',(-1.,0.,0.));
#17562=DIRECTION('ref_axis',(0.,0.660980889208583,-0.750402734603914));
#17563=DIRECTION('center_axis',(1.,0.,0.));
#17564=DIRECTION('ref_axis',(0.,0.707106781186548,-0.707106781186548));
#17565=DIRECTION('center_axis',(0.,-0.945990172710258,0.324195300915385));
#17566=DIRECTION('ref_axis',(1.,0.,0.));
#17567=DIRECTION('center_axis',(-1.,0.,0.));
#17568=DIRECTION('ref_axis',(0.,0.707106781186548,-0.707106781186548));
#17569=DIRECTION('center_axis',(1.,0.,0.));
#17570=DIRECTION('ref_axis',(0.,0.,-1.));
#17571=DIRECTION('center_axis',(1.,0.,0.));
#17572=DIRECTION('ref_axis',(0.,0.707106781186548,0.707106781186548));
#17573=DIRECTION('center_axis',(-1.,0.,0.));
#17574=DIRECTION('ref_axis',(0.,-0.178029704061997,-0.984025113740294));
#17575=DIRECTION('',(0.,-1.,0.));
#17576=DIRECTION('center_axis',(-1.,0.,0.));
#17577=DIRECTION('ref_axis',(0.,0.178029704061997,-0.984025113740294));
#17578=DIRECTION('center_axis',(1.,0.,0.));
#17579=DIRECTION('ref_axis',(0.,-0.707106781186547,0.707106781186548));
#17580=DIRECTION('center_axis',(-1.,0.,0.));
#17581=DIRECTION('ref_axis',(0.,0.939379515438772,-0.342879171099701));
#17582=DIRECTION('',(0.,-1.,0.));
#17583=DIRECTION('',(0.,0.,-1.));
#17584=DIRECTION('',(0.,1.,0.));
#17585=DIRECTION('center_axis',(-1.,0.,0.));
#17586=DIRECTION('ref_axis',(0.,0.939379515438772,0.342879171099701));
#17587=DIRECTION('center_axis',(1.,0.,0.));
#17588=DIRECTION('ref_axis',(0.,-0.707106781186548,-0.707106781186547));
#17589=DIRECTION('center_axis',(-1.,0.,0.));
#17590=DIRECTION('ref_axis',(0.,0.326047170834313,0.945353501284541));
#17591=DIRECTION('',(0.,1.,0.));
#17592=DIRECTION('center_axis',(-1.,0.,0.));
#17593=DIRECTION('ref_axis',(0.,-0.326047170834313,0.945353501284541));
#17594=DIRECTION('',(0.,1.,0.));
#17595=DIRECTION('',(0.,1.,0.));
#17596=DIRECTION('center_axis',(0.,1.,0.));
#17597=DIRECTION('ref_axis',(1.,0.,0.));
#17598=DIRECTION('center_axis',(0.,1.,0.));
#17599=DIRECTION('ref_axis',(1.,0.,0.));
#17600=DIRECTION('',(0.707106781186554,-0.707106781186541,-8.65956056235501E-17));
#17601=DIRECTION('center_axis',(0.,-1.,0.));
#17602=DIRECTION('ref_axis',(1.,0.,0.));
#17603=DIRECTION('center_axis',(0.,1.,0.));
#17604=DIRECTION('ref_axis',(-1.,0.,0.));
#17605=DIRECTION('',(0.,0.,-1.));
#17606=DIRECTION('',(-1.,0.,0.));
#17607=DIRECTION('',(0.,0.,1.));
#17608=DIRECTION('',(1.,0.,0.));
#17609=DIRECTION('center_axis',(0.,1.,0.));
#17610=DIRECTION('ref_axis',(1.,0.,0.));
#17611=DIRECTION('center_axis',(0.,1.,0.));
#17612=DIRECTION('ref_axis',(1.,0.,0.));
#17613=DIRECTION('center_axis',(0.,1.,0.));
#17614=DIRECTION('ref_axis',(1.,0.,0.));
#17615=DIRECTION('center_axis',(0.,1.,0.));
#17616=DIRECTION('ref_axis',(1.,0.,0.));
#17617=DIRECTION('center_axis',(0.,-1.,0.));
#17618=DIRECTION('ref_axis',(1.,0.,0.));
#17619=DIRECTION('',(0.,-1.,0.));
#17620=DIRECTION('center_axis',(0.,-1.,0.));
#17621=DIRECTION('ref_axis',(1.,0.,0.));
#17622=DIRECTION('center_axis',(0.,1.,0.));
#17623=DIRECTION('ref_axis',(1.,0.,0.));
#17624=DIRECTION('',(0.707106781186554,-0.707106781186541,-8.65956056235501E-17));
#17625=DIRECTION('center_axis',(0.,-1.,0.));
#17626=DIRECTION('ref_axis',(1.,0.,0.));
#17627=DIRECTION('center_axis',(0.,-1.,0.));
#17628=DIRECTION('ref_axis',(1.,0.,0.));
#17629=DIRECTION('',(0.,-1.,0.));
#17630=DIRECTION('center_axis',(0.,-1.,0.));
#17631=DIRECTION('ref_axis',(1.,0.,0.));
#17632=DIRECTION('center_axis',(0.,1.,0.));
#17633=DIRECTION('ref_axis',(1.,0.,0.));
#17634=DIRECTION('',(0.707106781186554,-0.707106781186541,-8.65956056235501E-17));
#17635=DIRECTION('center_axis',(0.,-1.,0.));
#17636=DIRECTION('ref_axis',(1.,0.,0.));
#17637=DIRECTION('center_axis',(0.,-1.,0.));
#17638=DIRECTION('ref_axis',(1.,0.,0.));
#17639=DIRECTION('',(0.,-1.,0.));
#17640=DIRECTION('center_axis',(0.,-1.,0.));
#17641=DIRECTION('ref_axis',(1.,0.,0.));
#17642=DIRECTION('center_axis',(0.,1.,0.));
#17643=DIRECTION('ref_axis',(1.,0.,0.));
#17644=DIRECTION('',(0.707106781186554,-0.707106781186541,-8.65956056235501E-17));
#17645=DIRECTION('center_axis',(0.,-1.,0.));
#17646=DIRECTION('ref_axis',(1.,0.,0.));
#17647=DIRECTION('center_axis',(0.,-1.,0.));
#17648=DIRECTION('ref_axis',(1.,0.,0.));
#17649=DIRECTION('',(0.,-1.,0.));
#17650=DIRECTION('center_axis',(0.,-1.,0.));
#17651=DIRECTION('ref_axis',(1.,0.,0.));
#17652=DIRECTION('center_axis',(0.,1.,0.));
#17653=DIRECTION('ref_axis',(1.,0.,0.));
#17654=DIRECTION('',(0.707106781186554,-0.707106781186541,-8.65956056235501E-17));
#17655=DIRECTION('center_axis',(0.,-1.,0.));
#17656=DIRECTION('ref_axis',(1.,0.,0.));
#17657=DIRECTION('center_axis',(0.,-1.,0.));
#17658=DIRECTION('ref_axis',(1.,0.,0.));
#17659=DIRECTION('',(0.,-1.,0.));
#17660=DIRECTION('center_axis',(0.,-1.,0.));
#17661=DIRECTION('ref_axis',(1.,0.,0.));
#17662=DIRECTION('center_axis',(0.,1.,0.));
#17663=DIRECTION('ref_axis',(0.718378767037319,0.,-0.695652173913042));
#17664=DIRECTION('center_axis',(1.,0.,0.));
#17665=DIRECTION('ref_axis',(0.,0.,-1.));
#17666=DIRECTION('center_axis',(1.,0.,0.));
#17667=DIRECTION('ref_axis',(0.,0.,-1.));
#17668=DIRECTION('',(1.,0.,0.));
#17669=DIRECTION('center_axis',(0.,-1.,0.));
#17670=DIRECTION('ref_axis',(-0.707106781186552,0.,-0.707106781186543));
#17671=DIRECTION('center_axis',(0.,-1.,0.));
#17672=DIRECTION('ref_axis',(-1.,0.,0.));
#17673=DIRECTION('',(0.,-1.,0.));
#17674=DIRECTION('',(0.,1.,0.));
#17675=DIRECTION('center_axis',(-0.408248290463861,-0.816496580927726,0.408248290463865));
#17676=DIRECTION('ref_axis',(-0.577350269189623,0.577350269189627,0.577350269189627));
#17677=DIRECTION('center_axis',(-1.,0.,0.));
#17678=DIRECTION('ref_axis',(0.,1.,0.));
#17679=DIRECTION('center_axis',(0.,0.,1.));
#17680=DIRECTION('ref_axis',(-1.,0.,0.));
#17681=DIRECTION('center_axis',(0.,1.,0.));
#17682=DIRECTION('ref_axis',(0.,0.,1.));
#17683=DIRECTION('center_axis',(0.,0.,1.));
#17684=DIRECTION('ref_axis',(-0.707106781186544,0.707106781186551,0.));
#17685=DIRECTION('center_axis',(0.,0.,1.));
#17686=DIRECTION('ref_axis',(0.,1.,0.));
#17687=DIRECTION('',(0.,0.,1.));
#17688=DIRECTION('center_axis',(0.,-1.,0.));
#17689=DIRECTION('ref_axis',(-0.707106781186546,0.,0.707106781186549));
#17690=DIRECTION('',(0.,1.,0.));
#17691=DIRECTION('',(0.,-1.,0.));
#17692=DIRECTION('center_axis',(-1.,0.,0.));
#17693=DIRECTION('ref_axis',(0.,0.707106781186549,0.707106781186546));
#17694=DIRECTION('center_axis',(-1.,0.,0.));
#17695=DIRECTION('ref_axis',(0.,0.,1.));
#17696=DIRECTION('',(1.,0.,0.));
#17697=DIRECTION('center_axis',(0.40824829046386,-0.40824829046386,-0.816496580927729));
#17698=DIRECTION('ref_axis',(-0.577350269189629,0.577350269189625,-0.577350269189623));
#17699=DIRECTION('center_axis',(-1.,0.,0.));
#17700=DIRECTION('ref_axis',(0.,0.70710678118655,-0.707106781186545));
#17701=DIRECTION('center_axis',(0.,1.,0.));
#17702=DIRECTION('ref_axis',(0.70710678118654,0.,0.707106781186555));
#17703=DIRECTION('center_axis',(0.,-1.,0.));
#17704=DIRECTION('ref_axis',(1.,0.,-2.22044604925032E-15));
#17705=DIRECTION('',(0.,-1.,0.));
#17706=DIRECTION('center_axis',(0.408248290463861,0.408248290463857,-0.81649658092773));
#17707=DIRECTION('ref_axis',(0.577350269189634,0.577350269189623,0.57735026918962));
#17708=DIRECTION('center_axis',(0.,0.,1.));
#17709=DIRECTION('ref_axis',(0.707106781186548,0.707106781186548,0.));
#17710=DIRECTION('center_axis',(0.,0.,1.));
#17711=DIRECTION('ref_axis',(1.,0.,0.));
#17712=DIRECTION('',(-1.,0.,0.));
#17713=DIRECTION('',(0.,1.,0.));
#17714=DIRECTION('',(1.,0.,0.));
#17715=DIRECTION('center_axis',(-1.,0.,0.));
#17716=DIRECTION('ref_axis',(0.,0.707106781186549,-0.707106781186546));
#17717=DIRECTION('center_axis',(-1.,0.,0.));
#17718=DIRECTION('ref_axis',(0.,1.,0.));
#17719=DIRECTION('center_axis',(0.,0.,1.));
#17720=DIRECTION('ref_axis',(0.707106781186551,0.707106781186544,0.));
#17721=DIRECTION('center_axis',(0.,0.,-1.));
#17722=DIRECTION('ref_axis',(0.707106781186548,0.707106781186548,0.));
#17723=DIRECTION('center_axis',(0.408248290463865,-0.816496580927724,-0.408248290463865));
#17724=DIRECTION('ref_axis',(-0.577350269189621,-0.577350269189628,0.577350269189628));
#17725=DIRECTION('center_axis',(0.,-1.,0.));
#17726=DIRECTION('ref_axis',(-1.,0.,0.));
#17727=DIRECTION('center_axis',(0.408248290463873,0.408248290463858,-0.816496580927724));
#17728=DIRECTION('ref_axis',(-0.577350269189634,-0.57735026918962,-0.577350269189623));
#17729=DIRECTION('center_axis',(-4.4408920985006E-15,-1.,0.));
#17730=DIRECTION('ref_axis',(0.,0.,-1.));
#17731=DIRECTION('center_axis',(-1.,0.,-8.88178419700124E-15));
#17732=DIRECTION('ref_axis',(0.,-1.,0.));
#17733=DIRECTION('center_axis',(0.,-1.,0.));
#17734=DIRECTION('ref_axis',(-0.707106781186554,0.,-0.707106781186541));
#17735=DIRECTION('',(0.,-1.,0.));
#17736=DIRECTION('',(0.,1.,0.));
#17737=DIRECTION('center_axis',(1.,0.,0.));
#17738=DIRECTION('ref_axis',(0.,-0.707106781186548,-0.707106781186548));
#17739=DIRECTION('',(1.,0.,0.));
#17740=DIRECTION('center_axis',(-1.,1.77635683940026E-14,0.));
#17741=DIRECTION('ref_axis',(0.,0.,-1.));
#17742=DIRECTION('',(-1.,0.,0.));
#17743=DIRECTION('center_axis',(-0.816496580927736,-0.408248290463854,-0.408248290463854));
#17744=DIRECTION('ref_axis',(0.577350269189608,-0.577350269189637,-0.577350269189633));
#17745=DIRECTION('center_axis',(0.,-1.,0.));
#17746=DIRECTION('ref_axis',(0.707106781186543,0.,-0.707106781186552));
#17747=DIRECTION('center_axis',(-0.81649658092773,-0.408248290463858,0.408248290463861));
#17748=DIRECTION('ref_axis',(0.577350269189622,-0.577350269189629,0.577350269189626));
#17749=DIRECTION('center_axis',(0.,-1.,0.));
#17750=DIRECTION('ref_axis',(0.707106781186543,0.,0.707106781186552));
#17751=DIRECTION('center_axis',(0.,-1.,0.));
#17752=DIRECTION('ref_axis',(-0.707106781186548,0.,0.707106781186548));
#17753=DIRECTION('',(0.,-1.,0.));
#17754=DIRECTION('',(0.,1.,0.));
#17755=DIRECTION('center_axis',(0.,1.,0.));
#17756=DIRECTION('ref_axis',(0.707106781186541,0.,-0.707106781186554));
#17757=DIRECTION('',(0.,1.,0.));
#17758=DIRECTION('center_axis',(0.,0.,1.));
#17759=DIRECTION('ref_axis',(1.,0.,0.));
#17760=DIRECTION('',(-1.,0.,0.));
#17761=DIRECTION('center_axis',(0.,-1.,0.));
#17762=DIRECTION('ref_axis',(1.,0.,0.));
#17763=DIRECTION('center_axis',(1.,0.,0.));
#17764=DIRECTION('ref_axis',(0.,0.,-1.));
#17765=DIRECTION('center_axis',(1.,0.,0.));
#17766=DIRECTION('ref_axis',(0.,0.694365074829414,-0.719622917128924));
#17767=DIRECTION('',(0.,1.,0.));
#17768=DIRECTION('center_axis',(1.,0.,0.));
#17769=DIRECTION('ref_axis',(0.,-0.566946709513841,-0.823754471047914));
#17770=DIRECTION('center_axis',(1.,0.,0.));
#17771=DIRECTION('ref_axis',(0.,-0.566946709513841,0.823754471047914));
#17772=DIRECTION('',(0.,-1.,0.));
#17773=DIRECTION('center_axis',(1.,0.,0.));
#17774=DIRECTION('ref_axis',(0.,0.694365074829414,0.719622917128924));
#17775=DIRECTION('center_axis',(-1.,0.,0.));
#17776=DIRECTION('ref_axis',(0.,1.,0.));
#17777=DIRECTION('center_axis',(1.,0.,0.));
#17778=DIRECTION('ref_axis',(0.,0.,-1.));
#17779=DIRECTION('center_axis',(1.,0.,0.));
#17780=DIRECTION('ref_axis',(0.,0.,-1.));
#17781=DIRECTION('center_axis',(1.,0.,0.));
#17782=DIRECTION('ref_axis',(0.,0.,-1.));
#17783=DIRECTION('center_axis',(1.,0.,0.));
#17784=DIRECTION('ref_axis',(0.,0.,-1.));
#17785=DIRECTION('center_axis',(1.,0.,0.));
#17786=DIRECTION('ref_axis',(0.,0.,-1.));
#17787=DIRECTION('center_axis',(0.,-1.,-1.22464679914735E-16));
#17788=DIRECTION('ref_axis',(0.,-1.22464679914735E-16,1.));
#17789=DIRECTION('center_axis',(1.,0.,0.));
#17790=DIRECTION('ref_axis',(0.,1.,0.));
#17791=DIRECTION('center_axis',(1.,0.,0.));
#17792=DIRECTION('ref_axis',(0.,1.,0.));
#17793=DIRECTION('center_axis',(1.,0.,0.));
#17794=DIRECTION('ref_axis',(0.,1.,0.));
#17795=DIRECTION('',(1.,0.,0.));
#17796=DIRECTION('center_axis',(1.,0.,0.));
#17797=DIRECTION('ref_axis',(0.,0.,-1.));
#17798=DIRECTION('center_axis',(1.,0.,0.));
#17799=DIRECTION('ref_axis',(0.,0.,-1.));
#17800=DIRECTION('center_axis',(0.,-1.,0.));
#17801=DIRECTION('ref_axis',(-1.,0.,0.));
#17802=DIRECTION('center_axis',(-1.,0.,0.));
#17803=DIRECTION('ref_axis',(0.,-0.566946709513841,-0.823754471047914));
#17804=DIRECTION('center_axis',(0.,1.,0.));
#17805=DIRECTION('ref_axis',(-0.707106781186544,0.,-0.707106781186551));
#17806=DIRECTION('center_axis',(0.,-1.,2.22044604925031E-15));
#17807=DIRECTION('ref_axis',(-1.,0.,0.));
#17808=DIRECTION('',(0.,-1.,0.));
#17809=DIRECTION('center_axis',(1.,0.,0.));
#17810=DIRECTION('ref_axis',(0.,0.,-1.));
#17811=DIRECTION('center_axis',(-1.,0.,0.));
#17812=DIRECTION('ref_axis',(0.,0.694365074829414,-0.719622917128924));
#17813=DIRECTION('center_axis',(0.,-1.,1.63845976266357E-14));
#17814=DIRECTION('ref_axis',(0.316350739523702,1.55431223447523E-14,0.948642298025345));
#17815=DIRECTION('center_axis',(0.,-1.304735096307E-15,1.));
#17816=DIRECTION('ref_axis',(-1.,0.,0.));
#17817=DIRECTION('center_axis',(1.,0.,0.));
#17818=DIRECTION('ref_axis',(0.,0.,-1.));
#17819=DIRECTION('center_axis',(1.,0.,0.));
#17820=DIRECTION('ref_axis',(0.,0.,-1.));
#17821=DIRECTION('center_axis',(1.,0.,0.));
#17822=DIRECTION('ref_axis',(0.,0.,-1.));
#17823=DIRECTION('center_axis',(1.,0.,0.));
#17824=DIRECTION('ref_axis',(0.,-0.704542565014449,-0.709661732153327));
#17825=DIRECTION('center_axis',(-1.,0.,0.));
#17826=DIRECTION('ref_axis',(0.,-0.704542565014449,-0.709661732153327));
#17827=DIRECTION('center_axis',(1.,0.,0.));
#17828=DIRECTION('ref_axis',(0.,0.,-1.));
#17829=DIRECTION('center_axis',(-1.,0.,0.));
#17830=DIRECTION('ref_axis',(0.,-0.999903350347485,0.0139028761007986));
#17831=DIRECTION('center_axis',(-1.,0.,0.));
#17832=DIRECTION('ref_axis',(0.,0.,-1.));
#17833=DIRECTION('center_axis',(-1.,0.,0.));
#17834=DIRECTION('ref_axis',(0.,0.,-1.));
#17835=DIRECTION('center_axis',(1.,0.,0.));
#17836=DIRECTION('ref_axis',(0.,0.,-1.));
#17837=DIRECTION('center_axis',(-1.,0.,0.));
#17838=DIRECTION('ref_axis',(0.,-0.704542565014449,0.709661732153327));
#17839=DIRECTION('center_axis',(1.,0.,0.));
#17840=DIRECTION('ref_axis',(0.,-0.704542565014449,0.709661732153327));
#17841=DIRECTION('center_axis',(1.,0.,0.));
#17842=DIRECTION('ref_axis',(0.,-1.58603289232165E-16,1.));
#17843=DIRECTION('',(-1.,0.,0.));
#17844=DIRECTION('center_axis',(1.,0.,0.));
#17845=DIRECTION('ref_axis',(0.,-0.326047170834313,0.945353501284541));
#17846=DIRECTION('',(1.,0.,0.));
#17847=DIRECTION('center_axis',(-1.,0.,0.));
#17848=DIRECTION('ref_axis',(0.,-0.566946709513841,0.823754471047914));
#17849=DIRECTION('',(1.,0.,0.));
#17850=DIRECTION('center_axis',(-1.,0.,0.));
#17851=DIRECTION('ref_axis',(0.,0.,1.));
#17852=DIRECTION('center_axis',(-1.,0.,0.));
#17853=DIRECTION('ref_axis',(0.,0.707106781186547,-0.707106781186548));
#17854=DIRECTION('center_axis',(1.,0.,0.));
#17855=DIRECTION('ref_axis',(0.,0.707106781186547,-0.707106781186548));
#17856=DIRECTION('center_axis',(1.,0.,0.));
#17857=DIRECTION('ref_axis',(0.,0.,-1.));
#17858=DIRECTION('center_axis',(-1.,0.,0.));
#17859=DIRECTION('ref_axis',(0.,-0.0139028761007986,-0.999903350347485));
#17860=DIRECTION('center_axis',(-1.,0.,0.));
#17861=DIRECTION('ref_axis',(0.,0.,-1.));
#17862=DIRECTION('center_axis',(-1.,0.,0.));
#17863=DIRECTION('ref_axis',(0.,0.999903350347485,0.0139028761007986));
#17864=DIRECTION('center_axis',(-1.,0.,0.));
#17865=DIRECTION('ref_axis',(0.,0.,-1.));
#17866=DIRECTION('center_axis',(-1.,0.,0.));
#17867=DIRECTION('ref_axis',(0.,0.,1.));
#17868=DIRECTION('center_axis',(-1.,0.,0.));
#17869=DIRECTION('ref_axis',(0.,0.707106781186548,0.707106781186547));
#17870=DIRECTION('center_axis',(1.,0.,0.));
#17871=DIRECTION('ref_axis',(0.,0.707106781186548,0.707106781186547));
#17872=DIRECTION('center_axis',(1.,0.,0.));
#17873=DIRECTION('ref_axis',(0.,0.,-1.));
#17874=DIRECTION('center_axis',(-1.,0.,0.));
#17875=DIRECTION('ref_axis',(0.,0.999903350347485,-0.0139028761007986));
#17876=DIRECTION('center_axis',(-1.,0.,0.));
#17877=DIRECTION('ref_axis',(0.,0.,-1.));
#17878=DIRECTION('center_axis',(-1.,0.,0.));
#17879=DIRECTION('ref_axis',(0.,-0.0139028761007986,0.999903350347485));
#17880=DIRECTION('center_axis',(-1.,0.,0.));
#17881=DIRECTION('ref_axis',(0.,0.,-1.));
#17882=DIRECTION('center_axis',(0.,-1.,0.));
#17883=DIRECTION('ref_axis',(-0.707106781186544,0.,0.707106781186551));
#17884=DIRECTION('center_axis',(0.,-1.,0.));
#17885=DIRECTION('ref_axis',(0.,0.,1.));
#17886=DIRECTION('center_axis',(0.,1.,-2.22044604925031E-15));
#17887=DIRECTION('ref_axis',(-1.,0.,0.));
#17888=DIRECTION('',(0.,1.,0.));
#17889=DIRECTION('center_axis',(1.,0.,0.));
#17890=DIRECTION('ref_axis',(0.,0.,-1.));
#17891=DIRECTION('center_axis',(1.,0.,0.));
#17892=DIRECTION('ref_axis',(0.,0.,-1.));
#17893=DIRECTION('center_axis',(-1.,0.,0.));
#17894=DIRECTION('ref_axis',(0.,0.694365074829414,0.719622917128924));
#17895=DIRECTION('center_axis',(1.,0.,0.));
#17896=DIRECTION('ref_axis',(0.,1.,1.58603289232165E-16));
#17897=DIRECTION('',(-1.,0.,0.));
#17898=DIRECTION('center_axis',(1.,0.,0.));
#17899=DIRECTION('ref_axis',(0.,0.939379515438772,0.342879171099701));
#17900=DIRECTION('',(-1.,0.,0.));
#17901=DIRECTION('',(1.,0.,0.));
#17902=DIRECTION('center_axis',(1.,0.,0.));
#17903=DIRECTION('ref_axis',(0.,0.326047170834313,0.945353501284541));
#17904=DIRECTION('',(1.,0.,0.));
#17905=DIRECTION('center_axis',(0.,0.,1.));
#17906=DIRECTION('ref_axis',(0.,-1.,0.));
#17907=DIRECTION('',(0.,-1.,0.));
#17908=DIRECTION('center_axis',(1.,0.,0.));
#17909=DIRECTION('ref_axis',(0.,0.,-1.));
#17910=DIRECTION('center_axis',(0.,-1.,0.));
#17911=DIRECTION('ref_axis',(0.,0.,-1.));
#17912=DIRECTION('center_axis',(-1.55596157992435E-15,0.936610848943197,
-0.35037139957751));
#17913=DIRECTION('ref_axis',(1.,0.,-4.44089209850056E-15));
#17914=DIRECTION('center_axis',(1.,0.,0.));
#17915=DIRECTION('ref_axis',(0.,-0.178029704061997,-0.984025113740294));
#17916=DIRECTION('center_axis',(0.,1.,0.));
#17917=DIRECTION('ref_axis',(0.707106781186538,0.,-0.707106781186557));
#17918=DIRECTION('center_axis',(0.,-1.,2.22044604925031E-15));
#17919=DIRECTION('ref_axis',(0.,-2.22044604925031E-15,-1.));
#17920=DIRECTION('',(0.,1.,0.));
#17921=DIRECTION('center_axis',(1.,0.,0.));
#17922=DIRECTION('ref_axis',(0.,0.,-1.));
#17923=DIRECTION('center_axis',(2.60342613851738E-15,-0.936610848943196,
-0.350371399577514));
#17924=DIRECTION('ref_axis',(0.,0.350371399577514,-0.936610848943196));
#17925=DIRECTION('center_axis',(1.,0.,0.));
#17926=DIRECTION('ref_axis',(0.,0.178029704061997,-0.984025113740294));
#17927=DIRECTION('center_axis',(0.,0.,1.));
#17928=DIRECTION('ref_axis',(1.,0.,0.));
#17929=DIRECTION('center_axis',(1.,0.,0.));
#17930=DIRECTION('ref_axis',(0.,0.999903350347485,0.0139028761007998));
#17931=DIRECTION('center_axis',(0.,0.945990172710257,-0.324195300915386));
#17932=DIRECTION('ref_axis',(0.,-0.324195300915386,-0.945990172710257));
#17933=DIRECTION('center_axis',(0.,0.,1.));
#17934=DIRECTION('ref_axis',(1.,0.,0.));
#17935=DIRECTION('center_axis',(0.,-0.945990172710257,-0.324195300915386));
#17936=DIRECTION('ref_axis',(0.,0.324195300915386,-0.945990172710257));
#17937=DIRECTION('center_axis',(1.,0.,0.));
#17938=DIRECTION('ref_axis',(0.,-0.999903350347485,0.0139028761007998));
#17939=DIRECTION('center_axis',(-1.,0.,0.));
#17940=DIRECTION('ref_axis',(0.,0.,1.));
#17941=DIRECTION('center_axis',(-1.,0.,0.));
#17942=DIRECTION('ref_axis',(0.,-0.707106781186547,0.707106781186548));
#17943=DIRECTION('center_axis',(0.,0.324195300915385,-0.945990172710258));
#17944=DIRECTION('ref_axis',(0.,-0.945990172710258,-0.324195300915385));
#17945=DIRECTION('center_axis',(1.,0.,0.));
#17946=DIRECTION('ref_axis',(0.,0.999903350347485,0.0139028761007986));
#17947=DIRECTION('',(-1.,0.,0.));
#17948=DIRECTION('',(1.,0.,0.));
#17949=DIRECTION('center_axis',(1.,0.,0.));
#17950=DIRECTION('ref_axis',(0.,1.58603289232165E-16,-1.));
#17951=DIRECTION('center_axis',(1.,0.,0.));
#17952=DIRECTION('ref_axis',(0.,0.939379515438772,-0.342879171099701));
#17953=DIRECTION('',(1.,0.,0.));
#17954=DIRECTION('',(1.,0.,0.));
#17955=DIRECTION('center_axis',(0.,0.,-1.));
#17956=DIRECTION('ref_axis',(0.,1.,0.));
#17957=DIRECTION('',(1.,0.,0.));
#17958=DIRECTION('center_axis',(1.,0.,0.));
#17959=DIRECTION('ref_axis',(0.,-1.,-1.58603289232165E-16));
#17960=DIRECTION('',(1.,0.,0.));
#17961=DIRECTION('center_axis',(0.,1.,0.));
#17962=DIRECTION('ref_axis',(0.707106781186541,0.,0.707106781186554));
#17963=DIRECTION('',(0.,-1.,0.));
#17964=DIRECTION('center_axis',(0.,0.,1.));
#17965=DIRECTION('ref_axis',(1.,0.,0.));
#17966=DIRECTION('',(1.,0.,0.));
#17967=DIRECTION('center_axis',(0.,1.,0.));
#17968=DIRECTION('ref_axis',(0.70710678118654,0.,-0.707106781186555));
#17969=DIRECTION('center_axis',(0.,-1.,0.));
#17970=DIRECTION('ref_axis',(0.,0.,-1.));
#17971=DIRECTION('center_axis',(-0.408248290463861,-0.408248290463847,-0.816496580927735));
#17972=DIRECTION('ref_axis',(0.577350269189648,0.577350269189616,-0.577350269189614));
#17973=DIRECTION('center_axis',(-1.,0.,0.));
#17974=DIRECTION('ref_axis',(0.,0.,1.));
#17975=DIRECTION('center_axis',(-1.,0.,0.));
#17976=DIRECTION('ref_axis',(0.,0.707106781186548,0.707106781186548));
#17977=DIRECTION('center_axis',(-1.,0.,0.));
#17978=DIRECTION('ref_axis',(0.,-0.999903350347485,0.0139028761007986));
#17979=DIRECTION('',(-1.,0.,0.));
#17980=DIRECTION('center_axis',(1.,0.,0.));
#17981=DIRECTION('ref_axis',(0.,0.946352857512202,0.323135063214268));
#17982=DIRECTION('',(-1.,0.,0.));
#17983=DIRECTION('center_axis',(-1.,0.,0.));
#17984=DIRECTION('ref_axis',(0.,0.946352857512202,0.323135063214268));
#17985=DIRECTION('center_axis',(-1.,0.,0.));
#17986=DIRECTION('ref_axis',(0.,0.,-1.));
#17987=DIRECTION('',(1.,0.,0.));
#17988=DIRECTION('center_axis',(-1.,0.,0.));
#17989=DIRECTION('ref_axis',(0.,0.,-1.));
#17990=DIRECTION('center_axis',(0.559184554883702,-0.00524477298579031,
-0.829026613526878));
#17991=DIRECTION('ref_axis',(0.828990150486439,-0.00777536702111098,0.559209150554744));
#17992=DIRECTION('center_axis',(1.,0.,0.));
#17993=DIRECTION('ref_axis',(0.,-0.945990172710258,0.324195300915385));
#17994=DIRECTION('center_axis',(0.,0.324195300915381,0.945990172710259));
#17995=DIRECTION('ref_axis',(1.,0.,0.));
#17996=DIRECTION('center_axis',(-4.15938771844182E-15,-0.350371399577514,
0.936610848943196));
#17997=DIRECTION('ref_axis',(0.,0.936610848943196,0.350371399577514));
#17998=DIRECTION('center_axis',(0.,0.,1.));
#17999=DIRECTION('ref_axis',(1.,0.,0.));
#18000=DIRECTION('center_axis',(1.,0.,0.));
#18001=DIRECTION('ref_axis',(0.,0.350371399577514,0.936610848943196));
#18002=DIRECTION('center_axis',(0.,0.936610848943196,-0.350371399577514));
#18003=DIRECTION('ref_axis',(1.,0.,0.));
#18004=DIRECTION('center_axis',(0.,0.945990172710258,0.324195300915385));
#18005=DIRECTION('ref_axis',(0.,0.324195300915385,-0.945990172710258));
#18006=DIRECTION('center_axis',(0.,0.,1.));
#18007=DIRECTION('ref_axis',(1.,0.,0.));
#18008=DIRECTION('center_axis',(1.,0.,0.));
#18009=DIRECTION('ref_axis',(0.,-0.324195300915385,-0.945990172710258));
#18010=DIRECTION('center_axis',(0.,-0.936610848943197,-0.35037139957751));
#18011=DIRECTION('ref_axis',(0.,-0.35037139957751,0.936610848943197));
#18012=DIRECTION('center_axis',(1.,0.,0.));
#18013=DIRECTION('ref_axis',(0.,0.,-1.));
#18014=DIRECTION('center_axis',(0.,1.,-2.22044604925031E-15));
#18015=DIRECTION('ref_axis',(0.,2.22044604925031E-15,1.));
#18016=DIRECTION('center_axis',(0.,-1.,0.));
#18017=DIRECTION('ref_axis',(0.707106781186538,0.,0.707106781186557));
#18018=DIRECTION('center_axis',(0.,1.,-2.22044604925031E-15));
#18019=DIRECTION('ref_axis',(0.,2.22044604925031E-15,1.));
#18020=DIRECTION('center_axis',(1.,0.,0.));
#18021=DIRECTION('ref_axis',(0.,0.,-1.));
#18022=DIRECTION('center_axis',(1.,0.,0.));
#18023=DIRECTION('ref_axis',(0.,-0.999903350347485,-0.0139028761007986));
#18024=DIRECTION('center_axis',(-1.,0.,0.));
#18025=DIRECTION('ref_axis',(0.,-0.999903350347485,-0.0139028761007986));
#18026=DIRECTION('center_axis',(-1.,0.,0.));
#18027=DIRECTION('ref_axis',(0.,-0.707106781186548,-0.707106781186548));
#18028=DIRECTION('center_axis',(-1.,0.,0.));
#18029=DIRECTION('ref_axis',(0.,-0.707106781186548,-0.707106781186547));
#18030=DIRECTION('center_axis',(-1.,0.,0.));
#18031=DIRECTION('ref_axis',(0.,0.999903350347485,-0.0139028761007986));
#18032=DIRECTION('',(-1.,0.,0.));
#18033=DIRECTION('center_axis',(1.,0.,0.));
#18034=DIRECTION('ref_axis',(0.,0.,-1.));
#18035=DIRECTION('center_axis',(1.,0.,0.));
#18036=DIRECTION('ref_axis',(0.,-0.0139028761007986,0.999903350347485));
#18037=DIRECTION('',(1.,0.,0.));
#18038=DIRECTION('center_axis',(-1.,0.,0.));
#18039=DIRECTION('ref_axis',(0.,0.,-1.));
#18040=DIRECTION('center_axis',(-0.559184554883714,0.00524477298580095,
-0.82902661352687));
#18041=DIRECTION('ref_axis',(0.828990150486434,-0.0077753670211287,-0.559209150554751));
#18042=DIRECTION('center_axis',(1.,0.,0.));
#18043=DIRECTION('ref_axis',(0.,0.936610848943196,-0.350371399577514));
#18044=DIRECTION('center_axis',(0.,-0.350371399577516,-0.936610848943195));
#18045=DIRECTION('ref_axis',(1.,0.,0.));
#18046=DIRECTION('center_axis',(1.,0.,0.));
#18047=DIRECTION('ref_axis',(0.,0.,-1.));
#18048=DIRECTION('center_axis',(-1.,0.,0.));
#18049=DIRECTION('ref_axis',(0.,-0.0139028761007986,-0.999903350347485));
#18050=DIRECTION('',(-1.,0.,0.));
#18051=DIRECTION('center_axis',(-1.,0.,0.));
#18052=DIRECTION('ref_axis',(0.,0.,-1.));
#18053=DIRECTION('',(-1.,0.,0.));
#18054=DIRECTION('center_axis',(-1.,0.,0.));
#18055=DIRECTION('ref_axis',(0.,0.,-1.));
#18056=DIRECTION('center_axis',(-1.,0.,0.));
#18057=DIRECTION('ref_axis',(0.,0.,-1.));
#18058=DIRECTION('',(-1.,0.,0.));
#18059=DIRECTION('center_axis',(-1.,0.,0.));
#18060=DIRECTION('ref_axis',(0.,0.,-1.));
#18061=DIRECTION('',(-1.,0.,0.));
#18062=DIRECTION('center_axis',(-1.,0.,0.));
#18063=DIRECTION('ref_axis',(0.,0.,-1.));
#18064=DIRECTION('',(-1.,0.,0.));
#18065=DIRECTION('center_axis',(-1.,0.,0.));
#18066=DIRECTION('ref_axis',(0.,-0.707106781186548,0.707106781186547));
#18067=DIRECTION('center_axis',(1.,0.,0.));
#18068=DIRECTION('ref_axis',(0.,0.,-1.));
#18069=DIRECTION('center_axis',(-1.,0.,0.));
#18070=DIRECTION('ref_axis',(0.,0.706710494065816,0.707502846338621));
#18071=DIRECTION('center_axis',(0.,1.,0.));
#18072=DIRECTION('ref_axis',(1.,0.,0.));
#18073=DIRECTION('center_axis',(0.,1.,0.));
#18074=DIRECTION('ref_axis',(1.,0.,0.));
#18075=DIRECTION('center_axis',(0.,1.,0.));
#18076=DIRECTION('ref_axis',(1.,0.,0.));
#18077=DIRECTION('center_axis',(0.,1.,0.));
#18078=DIRECTION('ref_axis',(1.,0.,0.));
#18079=DIRECTION('center_axis',(0.,1.,0.));
#18080=DIRECTION('ref_axis',(1.,0.,0.));
#18081=DIRECTION('center_axis',(0.,1.,0.));
#18082=DIRECTION('ref_axis',(1.,0.,0.));
#18083=DIRECTION('center_axis',(0.,1.,0.));
#18084=DIRECTION('ref_axis',(1.,0.,0.));
#18085=DIRECTION('center_axis',(0.,1.,0.));
#18086=DIRECTION('ref_axis',(1.,0.,0.));
#18087=DIRECTION('center_axis',(0.,1.,0.));
#18088=DIRECTION('ref_axis',(1.,0.,0.));
#18089=DIRECTION('center_axis',(0.,1.,0.));
#18090=DIRECTION('ref_axis',(1.,0.,0.));
#18091=DIRECTION('center_axis',(1.,0.,0.));
#18092=DIRECTION('ref_axis',(0.,1.,0.));
#18093=DIRECTION('',(1.,0.,0.));
#18094=DIRECTION('center_axis',(1.,0.,0.));
#18095=DIRECTION('ref_axis',(0.,0.,-1.));
#18096=DIRECTION('center_axis',(1.,0.,0.));
#18097=DIRECTION('ref_axis',(0.,0.,-1.));
#18098=DIRECTION('center_axis',(1.,0.,0.));
#18099=DIRECTION('ref_axis',(0.,0.,-1.));
#18100=DIRECTION('center_axis',(1.,0.,0.));
#18101=DIRECTION('ref_axis',(0.,1.,0.));
#18102=DIRECTION('',(1.,0.,0.));
#18103=DIRECTION('center_axis',(1.,0.,0.));
#18104=DIRECTION('ref_axis',(0.,0.,-1.));
#18105=DIRECTION('center_axis',(0.,0.,1.));
#18106=DIRECTION('ref_axis',(1.,0.,0.));
#18107=DIRECTION('axis',(0.,0.,1.));
#18108=DIRECTION('refdir',(1.,0.,0.));
#18109=DIRECTION('center_axis',(-0.707106781186546,-0.707106781186549,0.));
#18110=DIRECTION('ref_axis',(0.,0.,1.));
#18111=DIRECTION('center_axis',(-0.707106781186546,-0.707106781186549,0.));
#18112=DIRECTION('ref_axis',(-0.707106781186549,0.707106781186546,0.));
#18113=DIRECTION('',(0.,0.,1.));
#18114=DIRECTION('center_axis',(-0.707106781186546,-0.707106781186549,0.));
#18115=DIRECTION('ref_axis',(-0.707106781186549,0.707106781186546,0.));
#18116=DIRECTION('',(0.,0.,-1.));
#18117=DIRECTION('center_axis',(0.,-1.,0.));
#18118=DIRECTION('ref_axis',(0.,0.,-1.));
#18119=DIRECTION('',(1.,0.,0.));
#18120=DIRECTION('',(0.309016994374947,0.,-0.951056516295154));
#18121=DIRECTION('',(-1.,0.,0.));
#18122=DIRECTION('center_axis',(1.,0.,0.));
#18123=DIRECTION('ref_axis',(0.,1.,0.));
#18124=DIRECTION('center_axis',(-1.,0.,0.));
#18125=DIRECTION('ref_axis',(0.,1.,0.));
#18126=DIRECTION('center_axis',(-0.707106781186546,0.707106781186549,0.));
#18127=DIRECTION('ref_axis',(0.707106781186549,0.707106781186546,0.));
#18128=DIRECTION('',(-1.,0.,0.));
#18129=DIRECTION('center_axis',(0.672498511963957,0.707106781186548,0.21850801222441));
#18130=DIRECTION('ref_axis',(-0.740098474127776,0.6425202520624,0.198549677117357));
#18131=DIRECTION('center_axis',(0.951056516295154,0.,0.309016994374947));
#18132=DIRECTION('ref_axis',(-0.309016994374947,0.,0.951056516295154));
#18133=DIRECTION('center_axis',(0.672498511963957,-0.707106781186548,0.21850801222441));
#18134=DIRECTION('ref_axis',(0.740098474127776,0.6425202520624,-0.198549677117357));
#18135=DIRECTION('center_axis',(0.672498511963957,-0.707106781186548,0.21850801222441));
#18136=DIRECTION('ref_axis',(0.309016994374947,0.,-0.951056516295154));
#18137=DIRECTION('center_axis',(0.672498511963957,-0.707106781186548,0.21850801222441));
#18138=DIRECTION('ref_axis',(0.740098474127776,0.6425202520624,-0.198549677117357));
#18139=DIRECTION('',(-0.309016994374947,0.,0.951056516295154));
#18140=DIRECTION('center_axis',(0.951056516295154,0.,0.309016994374947));
#18141=DIRECTION('ref_axis',(0.309016994374947,0.,-0.951056516295154));
#18142=DIRECTION('',(0.309016994374947,0.,-0.951056516295154));
#18143=DIRECTION('center_axis',(0.951056516295154,0.,0.309016994374947));
#18144=DIRECTION('ref_axis',(-0.309016994374947,0.,0.951056516295154));
#18145=DIRECTION('center_axis',(-0.951056516295154,0.,-0.309016994374947));
#18146=DIRECTION('ref_axis',(-0.309016994374947,0.,0.951056516295154));
#18147=DIRECTION('center_axis',(-0.707106781186546,0.707106781186549,0.));
#18148=DIRECTION('ref_axis',(0.,0.,1.));
#18149=DIRECTION('center_axis',(-0.707106781186546,0.707106781186549,0.));
#18150=DIRECTION('ref_axis',(0.707106781186549,0.707106781186546,0.));
#18151=DIRECTION('',(0.,0.,-1.));
#18152=DIRECTION('',(0.,0.,1.));
#18153=DIRECTION('center_axis',(-1.,0.,0.));
#18154=DIRECTION('ref_axis',(0.,0.,1.));
#18155=DIRECTION('center_axis',(-1.,0.,0.));
#18156=DIRECTION('ref_axis',(0.,1.,0.));
#18157=DIRECTION('center_axis',(1.,0.,0.));
#18158=DIRECTION('ref_axis',(0.,1.,0.));
#18159=DIRECTION('center_axis',(0.672498511963957,0.707106781186548,0.21850801222441));
#18160=DIRECTION('ref_axis',(0.309016994374947,0.,-0.951056516295154));
#18161=DIRECTION('',(-0.309016994374947,0.,0.951056516295154));
#18162=DIRECTION('center_axis',(0.672498511963957,0.707106781186548,0.21850801222441));
#18163=DIRECTION('ref_axis',(-0.740098474127776,0.6425202520624,0.198549677117357));
#18164=DIRECTION('center_axis',(1.,0.,0.));
#18165=DIRECTION('ref_axis',(0.,1.,0.));
#18166=DIRECTION('',(1.,0.,0.));
#18167=DIRECTION('center_axis',(1.,0.,0.));
#18168=DIRECTION('ref_axis',(0.,1.,0.));
#18169=DIRECTION('',(1.,0.,0.));
#18170=DIRECTION('center_axis',(0.,1.,0.));
#18171=DIRECTION('ref_axis',(0.,0.,1.));
#18172=DIRECTION('axis',(0.,0.,1.));
#18173=DIRECTION('refdir',(1.,0.,0.));
#18174=DIRECTION('center_axis',(1.,0.,-7.24866760671198E-15));
#18175=DIRECTION('ref_axis',(0.,-1.,-3.09315763145967E-17));
#18176=DIRECTION('center_axis',(-1.,0.,0.));
#18177=DIRECTION('ref_axis',(0.,-1.,-6.12323399573677E-17));
#18178=DIRECTION('center_axis',(-1.,0.,0.));
#18179=DIRECTION('ref_axis',(0.,-1.,-6.12323399573677E-17));
#18180=DIRECTION('',(-0.38268343236509,-0.923879532511287,2.63222533831604E-15));
#18181=DIRECTION('center_axis',(1.,0.,0.));
#18182=DIRECTION('ref_axis',(0.,-1.,0.));
#18183=DIRECTION('center_axis',(-1.,0.,0.));
#18184=DIRECTION('ref_axis',(0.,0.,1.));
#18185=DIRECTION('center_axis',(1.,0.,0.));
#18186=DIRECTION('ref_axis',(0.,0.,-1.));
#18187=DIRECTION('center_axis',(1.,0.,0.));
#18188=DIRECTION('ref_axis',(0.,0.78183148246803,-0.623489801858733));
#18189=DIRECTION('center_axis',(1.,0.,0.));
#18190=DIRECTION('ref_axis',(0.,0.974927912181824,0.222520933956314));
#18191=DIRECTION('center_axis',(1.,0.,0.));
#18192=DIRECTION('ref_axis',(0.,0.433883739117558,0.900968867902419));
#18193=DIRECTION('center_axis',(1.,0.,0.));
#18194=DIRECTION('ref_axis',(0.,-0.433883739117558,0.900968867902419));
#18195=DIRECTION('center_axis',(1.,0.,0.));
#18196=DIRECTION('ref_axis',(0.,-0.974927912181824,0.222520933956315));
#18197=DIRECTION('center_axis',(1.,0.,0.));
#18198=DIRECTION('ref_axis',(0.,-0.78183148246803,-0.623489801858733));
#18199=DIRECTION('',(0.,0.,1.));
#18200=DIRECTION('center_axis',(1.,0.,0.));
#18201=DIRECTION('ref_axis',(0.,0.,-1.));
#18202=DIRECTION('',(0.,0.,-1.));
#18203=DIRECTION('',(0.,1.,0.));
#18204=DIRECTION('center_axis',(1.,0.,0.));
#18205=DIRECTION('ref_axis',(0.,1.,0.));
#18206=DIRECTION('center_axis',(1.,0.,0.));
#18207=DIRECTION('ref_axis',(0.,0.,-1.));
#18208=DIRECTION('',(-0.707106781186548,0.707106781186548,8.65956056235493E-17));
#18209=DIRECTION('center_axis',(-0.707106781186555,0.70710678118654,0.));
#18210=DIRECTION('ref_axis',(0.,0.,1.));
#18211=DIRECTION('',(0.,0.,-1.));
#18212=DIRECTION('center_axis',(0.707106781186555,-0.70710678118654,0.));
#18213=DIRECTION('ref_axis',(0.70710678118654,0.707106781186555,0.));
#18214=DIRECTION('',(0.577350269189617,0.57735026918963,-0.57735026918963));
#18215=DIRECTION('center_axis',(-0.707106781186557,-0.707106781186538,0.));
#18216=DIRECTION('ref_axis',(0.,0.,1.));
#18217=DIRECTION('center_axis',(0.707106781186557,0.707106781186538,0.));
#18218=DIRECTION('ref_axis',(-0.707106781186538,0.707106781186557,0.));
#18219=DIRECTION('',(0.,0.,1.));
#18220=DIRECTION('',(-0.577350269189616,0.577350269189632,0.577350269189629));
#18221=DIRECTION('center_axis',(-0.707106781186543,0.,-0.707106781186552));
#18222=DIRECTION('ref_axis',(-0.707106781186552,0.,0.707106781186543));
#18223=DIRECTION('',(0.,-1.,0.));
#18224=DIRECTION('center_axis',(0.,-1.,0.));
#18225=DIRECTION('ref_axis',(1.,0.,0.));
#18226=DIRECTION('',(1.,0.,0.));
#18227=DIRECTION('',(0.,0.,1.));
#18228=DIRECTION('',(1.,0.,0.));
#18229=DIRECTION('center_axis',(0.,0.,1.));
#18230=DIRECTION('ref_axis',(1.,0.,0.));
#18231=DIRECTION('',(-1.,0.,0.));
#18232=DIRECTION('',(0.,1.,0.));
#18233=DIRECTION('center_axis',(1.,0.,0.));
#18234=DIRECTION('ref_axis',(0.,-1.83697019872103E-16,-1.));
#18235=DIRECTION('center_axis',(-0.707106781186555,-0.70710678118654,0.));
#18236=DIRECTION('ref_axis',(-0.70710678118654,0.707106781186555,0.));
#18237=DIRECTION('center_axis',(1.,0.,0.));
#18238=DIRECTION('ref_axis',(0.,0.,-1.));
#18239=DIRECTION('center_axis',(-0.70710678118653,0.707106781186565,0.));
#18240=DIRECTION('ref_axis',(0.707106781186565,0.70710678118653,0.));
#18241=DIRECTION('',(-1.,0.,0.));
#18242=DIRECTION('center_axis',(0.,1.,0.));
#18243=DIRECTION('ref_axis',(-1.,0.,0.));
#18244=DIRECTION('',(0.,0.,-1.));
#18245=DIRECTION('center_axis',(0.707106781186555,0.70710678118654,0.));
#18246=DIRECTION('ref_axis',(0.,0.,-1.));
#18247=DIRECTION('',(0.,0.,-1.));
#18248=DIRECTION('',(0.577350269189617,-0.57735026918963,0.57735026918963));
#18249=DIRECTION('center_axis',(0.70710678118653,-0.707106781186565,0.));
#18250=DIRECTION('ref_axis',(0.,0.,-1.));
#18251=DIRECTION('',(0.,0.,1.));
#18252=DIRECTION('',(-0.577350269189631,-0.577350269189623,-0.577350269189623));
#18253=DIRECTION('center_axis',(0.707106781186543,0.,-0.707106781186552));
#18254=DIRECTION('ref_axis',(-0.707106781186552,0.,-0.707106781186543));
#18255=DIRECTION('',(0.,-1.,0.));
#18256=DIRECTION('center_axis',(1.,0.,0.));
#18257=DIRECTION('ref_axis',(0.,0.,-1.));
#18258=DIRECTION('center_axis',(1.,0.,0.));
#18259=DIRECTION('ref_axis',(0.,0.,-1.));
#18260=DIRECTION('center_axis',(-1.,0.,0.));
#18261=DIRECTION('ref_axis',(0.,0.,-1.));
#18262=DIRECTION('center_axis',(-1.,0.,0.));
#18263=DIRECTION('ref_axis',(0.,0.78183148246803,-0.623489801858734));
#18264=DIRECTION('center_axis',(-1.,0.,0.));
#18265=DIRECTION('ref_axis',(0.,0.974927912181824,0.222520933956314));
#18266=DIRECTION('center_axis',(-1.,0.,0.));
#18267=DIRECTION('ref_axis',(0.,0.433883739117558,0.900968867902419));
#18268=DIRECTION('center_axis',(-1.,0.,0.));
#18269=DIRECTION('ref_axis',(0.,-0.433883739117558,0.900968867902419));
#18270=DIRECTION('center_axis',(-1.,0.,0.));
#18271=DIRECTION('ref_axis',(0.,-0.974927912181824,0.222520933956315));
#18272=DIRECTION('center_axis',(-1.,0.,0.));
#18273=DIRECTION('ref_axis',(0.,-0.78183148246803,-0.623489801858733));
#18274=DIRECTION('center_axis',(-1.,0.,0.));
#18275=DIRECTION('ref_axis',(0.,-0.78183148246803,-0.623489801858733));
#18276=DIRECTION('',(-1.,0.,0.));
#18277=DIRECTION('center_axis',(1.,0.,0.));
#18278=DIRECTION('ref_axis',(0.,-0.78183148246803,-0.623489801858733));
#18279=DIRECTION('center_axis',(1.,0.,0.));
#18280=DIRECTION('ref_axis',(0.,-0.78183148246803,-0.623489801858733));
#18281=DIRECTION('',(1.,0.,0.));
#18282=DIRECTION('center_axis',(1.,0.,0.));
#18283=DIRECTION('ref_axis',(0.,-0.78183148246803,-0.623489801858733));
#18284=DIRECTION('center_axis',(1.,0.,0.));
#18285=DIRECTION('ref_axis',(0.,-0.78183148246803,-0.623489801858733));
#18286=DIRECTION('center_axis',(-1.,0.,0.));
#18287=DIRECTION('ref_axis',(0.,-0.974927912181824,0.222520933956315));
#18288=DIRECTION('',(-1.,0.,0.));
#18289=DIRECTION('center_axis',(1.,0.,0.));
#18290=DIRECTION('ref_axis',(0.,-0.974927912181824,0.222520933956315));
#18291=DIRECTION('center_axis',(1.,0.,0.));
#18292=DIRECTION('ref_axis',(0.,-0.974927912181824,0.222520933956315));
#18293=DIRECTION('',(1.,0.,0.));
#18294=DIRECTION('center_axis',(1.,0.,0.));
#18295=DIRECTION('ref_axis',(0.,-0.974927912181824,0.222520933956315));
#18296=DIRECTION('center_axis',(1.,0.,0.));
#18297=DIRECTION('ref_axis',(0.,-0.974927912181824,0.222520933956315));
#18298=DIRECTION('center_axis',(-1.,0.,0.));
#18299=DIRECTION('ref_axis',(0.,-0.433883739117558,0.900968867902419));
#18300=DIRECTION('',(-1.,0.,0.));
#18301=DIRECTION('center_axis',(1.,0.,0.));
#18302=DIRECTION('ref_axis',(0.,-0.433883739117558,0.900968867902419));
#18303=DIRECTION('center_axis',(1.,0.,0.));
#18304=DIRECTION('ref_axis',(0.,-0.433883739117558,0.900968867902419));
#18305=DIRECTION('',(1.,0.,0.));
#18306=DIRECTION('center_axis',(1.,0.,0.));
#18307=DIRECTION('ref_axis',(0.,-0.433883739117558,0.900968867902419));
#18308=DIRECTION('center_axis',(1.,0.,0.));
#18309=DIRECTION('ref_axis',(0.,-0.433883739117558,0.900968867902419));
#18310=DIRECTION('center_axis',(-1.,0.,0.));
#18311=DIRECTION('ref_axis',(0.,0.433883739117558,0.900968867902419));
#18312=DIRECTION('',(-1.,0.,0.));
#18313=DIRECTION('center_axis',(1.,0.,0.));
#18314=DIRECTION('ref_axis',(0.,0.433883739117558,0.900968867902419));
#18315=DIRECTION('center_axis',(1.,0.,0.));
#18316=DIRECTION('ref_axis',(0.,0.433883739117558,0.900968867902419));
#18317=DIRECTION('',(1.,0.,0.));
#18318=DIRECTION('center_axis',(1.,0.,0.));
#18319=DIRECTION('ref_axis',(0.,0.433883739117558,0.900968867902419));
#18320=DIRECTION('center_axis',(1.,0.,0.));
#18321=DIRECTION('ref_axis',(0.,0.433883739117558,0.900968867902419));
#18322=DIRECTION('center_axis',(-1.,0.,0.));
#18323=DIRECTION('ref_axis',(0.,0.974927912181824,0.222520933956314));
#18324=DIRECTION('',(-1.,0.,0.));
#18325=DIRECTION('center_axis',(1.,0.,0.));
#18326=DIRECTION('ref_axis',(0.,0.974927912181824,0.222520933956314));
#18327=DIRECTION('center_axis',(1.,0.,0.));
#18328=DIRECTION('ref_axis',(0.,0.974927912181824,0.222520933956314));
#18329=DIRECTION('',(1.,0.,0.));
#18330=DIRECTION('center_axis',(1.,0.,0.));
#18331=DIRECTION('ref_axis',(0.,0.974927912181824,0.222520933956314));
#18332=DIRECTION('center_axis',(1.,0.,0.));
#18333=DIRECTION('ref_axis',(0.,0.974927912181824,0.222520933956314));
#18334=DIRECTION('center_axis',(-1.,0.,0.));
#18335=DIRECTION('ref_axis',(0.,0.78183148246803,-0.623489801858734));
#18336=DIRECTION('',(-1.,0.,0.));
#18337=DIRECTION('center_axis',(1.,0.,0.));
#18338=DIRECTION('ref_axis',(0.,0.78183148246803,-0.623489801858734));
#18339=DIRECTION('center_axis',(1.,0.,0.));
#18340=DIRECTION('ref_axis',(0.,0.78183148246803,-0.623489801858733));
#18341=DIRECTION('',(1.,0.,0.));
#18342=DIRECTION('center_axis',(1.,0.,0.));
#18343=DIRECTION('ref_axis',(0.,0.78183148246803,-0.623489801858733));
#18344=DIRECTION('center_axis',(1.,0.,0.));
#18345=DIRECTION('ref_axis',(0.,0.78183148246803,-0.623489801858734));
#18346=DIRECTION('center_axis',(-1.,0.,0.));
#18347=DIRECTION('ref_axis',(0.,0.,-1.));
#18348=DIRECTION('',(-1.,0.,0.));
#18349=DIRECTION('center_axis',(1.,0.,0.));
#18350=DIRECTION('ref_axis',(0.,0.,-1.));
#18351=DIRECTION('center_axis',(1.,0.,0.));
#18352=DIRECTION('ref_axis',(0.,0.,-1.));
#18353=DIRECTION('',(1.,0.,0.));
#18354=DIRECTION('center_axis',(1.,0.,0.));
#18355=DIRECTION('ref_axis',(0.,0.,-1.));
#18356=DIRECTION('center_axis',(1.,0.,0.));
#18357=DIRECTION('ref_axis',(0.,0.,-1.));
#18358=DIRECTION('center_axis',(1.,0.,0.));
#18359=DIRECTION('ref_axis',(0.,1.,0.));
#18360=DIRECTION('',(-1.,0.,0.));
#18361=DIRECTION('axis',(0.,0.,1.));
#18362=DIRECTION('refdir',(1.,0.,0.));
#18363=DIRECTION('center_axis',(0.707106781186557,0.68301270189221,-0.183012701892217));
#18364=DIRECTION('ref_axis',(-0.250562807085725,0.,-0.968100345886377));
#18365=DIRECTION('center_axis',(0.707106781186557,0.68301270189221,-0.183012701892217));
#18366=DIRECTION('ref_axis',(-0.707106781186538,0.683012701892228,-0.183012701892222));
#18367=DIRECTION('',(0.,0.258819045102521,0.965925826289068));
#18368=DIRECTION('center_axis',(-0.707106781186557,-0.68301270189221,0.183012701892217));
#18369=DIRECTION('ref_axis',(-0.707106781186538,0.683012701892229,-0.183012701892222));
#18370=DIRECTION('',(0.,-0.258819045102521,-0.965925826289068));
#18371=DIRECTION('center_axis',(0.,-0.965925826289068,0.258819045102521));
#18372=DIRECTION('ref_axis',(0.,-0.258819045102521,-0.965925826289068));
#18373=DIRECTION('',(1.,0.,0.));
#18374=DIRECTION('',(0.,-0.258819045102521,-0.965925826289068));
#18375=DIRECTION('',(1.,0.,0.));
#18376=DIRECTION('center_axis',(-0.707106781186562,0.683012701892206,-0.183012701892215));
#18377=DIRECTION('ref_axis',(-0.250562807085722,0.,0.968100345886377));
#18378=DIRECTION('center_axis',(0.707106781186562,-0.683012701892206,0.183012701892215));
#18379=DIRECTION('ref_axis',(0.707106781186533,0.683012701892233,-0.183012701892223));
#18380=DIRECTION('center_axis',(-0.707106781186562,0.683012701892206,-0.183012701892215));
#18381=DIRECTION('ref_axis',(0.707106781186533,0.683012701892233,-0.183012701892223));
#18382=DIRECTION('',(0.,0.258819045102521,0.965925826289068));
#18383=DIRECTION('center_axis',(0.707106781186557,0.68301270189221,0.183012701892217));
#18384=DIRECTION('ref_axis',(0.250562807085726,0.,-0.968100345886376));
#18385=DIRECTION('center_axis',(-0.707106781186557,-0.68301270189221,-0.183012701892217));
#18386=DIRECTION('ref_axis',(-0.707106781186538,0.683012701892228,0.183012701892222));
#18387=DIRECTION('',(0.,-0.258819045102521,0.965925826289068));
#18388=DIRECTION('center_axis',(0.707106781186557,0.68301270189221,0.183012701892217));
#18389=DIRECTION('ref_axis',(-0.707106781186538,0.683012701892229,0.183012701892222));
#18390=DIRECTION('',(0.,0.258819045102521,-0.965925826289068));
#18391=DIRECTION('center_axis',(0.,-0.965925826289068,-0.258819045102521));
#18392=DIRECTION('ref_axis',(0.,0.258819045102521,-0.965925826289068));
#18393=DIRECTION('',(1.,0.,0.));
#18394=DIRECTION('',(0.,0.258819045102521,-0.965925826289068));
#18395=DIRECTION('',(1.,0.,0.));
#18396=DIRECTION('center_axis',(-0.707106781186556,0.683012701892211,0.183012701892217));
#18397=DIRECTION('ref_axis',(0.250562807085726,0.,0.968100345886376));
#18398=DIRECTION('center_axis',(-0.707106781186556,0.683012701892211,0.183012701892217));
#18399=DIRECTION('ref_axis',(0.707106781186539,0.683012701892228,0.183012701892222));
#18400=DIRECTION('center_axis',(0.707106781186556,-0.683012701892211,-0.183012701892217));
#18401=DIRECTION('ref_axis',(0.707106781186539,0.683012701892228,0.183012701892222));
#18402=DIRECTION('',(0.,-0.258819045102521,0.965925826289068));
#18403=DIRECTION('center_axis',(0.70710678118655,-0.683012701892217,0.183012701892219));
#18404=DIRECTION('ref_axis',(0.25056280708573,0.,-0.968100345886375));
#18405=DIRECTION('center_axis',(0.70710678118655,-0.683012701892217,0.183012701892219));
#18406=DIRECTION('ref_axis',(-0.707106781186545,-0.683012701892222,0.18301270189222));
#18407=DIRECTION('',(0.,-0.258819045102521,-0.965925826289068));
#18408=DIRECTION('center_axis',(-0.70710678118655,0.683012701892217,-0.183012701892219));
#18409=DIRECTION('ref_axis',(-0.707106781186545,-0.683012701892222,0.18301270189222));
#18410=DIRECTION('',(0.,0.258819045102521,0.965925826289068));
#18411=DIRECTION('center_axis',(0.,0.965925826289068,-0.258819045102521));
#18412=DIRECTION('ref_axis',(0.,0.258819045102521,0.965925826289068));
#18413=DIRECTION('',(1.,0.,0.));
#18414=DIRECTION('',(0.,0.258819045102521,0.965925826289068));
#18415=DIRECTION('',(1.,0.,0.));
#18416=DIRECTION('center_axis',(-0.70710678118655,-0.683012701892217,0.183012701892219));
#18417=DIRECTION('ref_axis',(0.25056280708573,0.,0.968100345886375));
#18418=DIRECTION('center_axis',(0.70710678118655,0.683012701892217,-0.183012701892219));
#18419=DIRECTION('ref_axis',(0.707106781186545,-0.683012701892222,0.18301270189222));
#18420=DIRECTION('center_axis',(-0.70710678118655,-0.683012701892217,0.183012701892219));
#18421=DIRECTION('ref_axis',(0.707106781186545,-0.683012701892222,0.18301270189222));
#18422=DIRECTION('',(0.,-0.258819045102521,-0.965925826289068));
#18423=DIRECTION('center_axis',(0.707106781186554,-0.683012701892213,-0.183012701892218));
#18424=DIRECTION('ref_axis',(-0.250562807085727,0.,-0.968100345886376));
#18425=DIRECTION('center_axis',(-0.707106781186554,0.683012701892213,0.183012701892218));
#18426=DIRECTION('ref_axis',(-0.707106781186541,-0.683012701892225,-0.183012701892221));
#18427=DIRECTION('',(0.,0.258819045102521,-0.965925826289068));
#18428=DIRECTION('center_axis',(0.707106781186554,-0.683012701892213,-0.183012701892218));
#18429=DIRECTION('ref_axis',(-0.707106781186541,-0.683012701892225,-0.183012701892221));
#18430=DIRECTION('',(0.,-0.258819045102521,0.965925826289068));
#18431=DIRECTION('center_axis',(0.,0.965925826289068,0.258819045102521));
#18432=DIRECTION('ref_axis',(0.,-0.258819045102521,0.965925826289068));
#18433=DIRECTION('',(1.,0.,0.));
#18434=DIRECTION('',(0.,-0.258819045102521,0.965925826289068));
#18435=DIRECTION('',(1.,0.,0.));
#18436=DIRECTION('center_axis',(-0.707106781186549,-0.683012701892218,-0.183012701892219));
#18437=DIRECTION('ref_axis',(-0.25056280708573,0.,0.968100345886375));
#18438=DIRECTION('center_axis',(-0.707106781186549,-0.683012701892218,-0.183012701892219));
#18439=DIRECTION('ref_axis',(0.707106781186546,-0.683012701892221,-0.18301270189222));
#18440=DIRECTION('center_axis',(0.707106781186549,0.683012701892218,0.183012701892219));
#18441=DIRECTION('ref_axis',(0.707106781186546,-0.683012701892221,-0.18301270189222));
#18442=DIRECTION('',(0.,0.258819045102521,-0.965925826289068));
#18443=DIRECTION('center_axis',(1.,0.,0.));
#18444=DIRECTION('ref_axis',(0.,-0.258819045102521,0.965925826289068));
#18445=DIRECTION('center_axis',(1.,0.,0.));
#18446=DIRECTION('ref_axis',(0.,-0.258819045102521,0.965925826289068));
#18447=DIRECTION('center_axis',(-1.,0.,0.));
#18448=DIRECTION('ref_axis',(0.,-0.258819045102521,0.965925826289068));
#18449=DIRECTION('center_axis',(1.,0.,0.));
#18450=DIRECTION('ref_axis',(0.,-0.258819045102521,0.965925826289068));
#18451=DIRECTION('center_axis',(-1.,0.,0.));
#18452=DIRECTION('ref_axis',(0.,-0.258819045102521,0.965925826289068));
#18453=DIRECTION('center_axis',(1.,0.,0.));
#18454=DIRECTION('ref_axis',(0.,-0.258819045102521,0.965925826289068));
#18455=DIRECTION('center_axis',(1.,0.,0.));
#18456=DIRECTION('ref_axis',(0.,0.258819045102521,-0.965925826289068));
#18457=DIRECTION('center_axis',(1.,0.,0.));
#18458=DIRECTION('ref_axis',(0.,0.258819045102521,-0.965925826289068));
#18459=DIRECTION('center_axis',(-1.,0.,0.));
#18460=DIRECTION('ref_axis',(0.,0.258819045102521,-0.965925826289068));
#18461=DIRECTION('center_axis',(1.,0.,0.));
#18462=DIRECTION('ref_axis',(0.,0.258819045102521,-0.965925826289068));
#18463=DIRECTION('center_axis',(-1.,0.,0.));
#18464=DIRECTION('ref_axis',(0.,0.258819045102521,-0.965925826289068));
#18465=DIRECTION('center_axis',(1.,0.,0.));
#18466=DIRECTION('ref_axis',(0.,0.258819045102521,-0.965925826289068));
#18467=DIRECTION('center_axis',(1.,0.,0.));
#18468=DIRECTION('ref_axis',(0.,1.,0.));
#18469=DIRECTION('center_axis',(1.,0.,0.));
#18470=DIRECTION('ref_axis',(0.,0.,-1.));
#18471=DIRECTION('',(-1.,0.,0.));
#18472=DIRECTION('center_axis',(1.,0.,0.));
#18473=DIRECTION('ref_axis',(0.,0.,-1.));
#18474=DIRECTION('center_axis',(-1.,0.,0.));
#18475=DIRECTION('ref_axis',(0.,0.,1.));
#18476=DIRECTION('center_axis',(1.,0.,0.));
#18477=DIRECTION('ref_axis',(0.,0.,-1.));
#18478=DIRECTION('center_axis',(1.,0.,0.));
#18479=DIRECTION('ref_axis',(0.,1.,0.));
#18480=DIRECTION('center_axis',(1.,0.,0.));
#18481=DIRECTION('ref_axis',(0.,0.,-1.));
#18482=DIRECTION('',(-1.,0.,0.));
#18483=DIRECTION('center_axis',(1.,0.,0.));
#18484=DIRECTION('ref_axis',(0.,0.,-1.));
#18485=DIRECTION('axis',(0.,0.,1.));
#18486=DIRECTION('refdir',(1.,0.,0.));
#18487=DIRECTION('center_axis',(0.,0.993813628552114,-0.111060666773081));
#18488=DIRECTION('ref_axis',(0.,0.111060666773081,0.993813628552114));
#18489=DIRECTION('',(-1.,0.,0.));
#18490=DIRECTION('',(1.,0.,0.));
#18491=DIRECTION('center_axis',(0.,0.248567642137747,0.968614540094294));
#18492=DIRECTION('ref_axis',(1.,0.,0.));
#18493=DIRECTION('',(-1.,0.,0.));
#18494=DIRECTION('',(1.,0.,0.));
#18495=DIRECTION('center_axis',(1.,0.,0.));
#18496=DIRECTION('ref_axis',(0.,1.,0.));
#18497=DIRECTION('center_axis',(-1.,0.,0.));
#18498=DIRECTION('ref_axis',(0.,1.,0.));
#18499=DIRECTION('center_axis',(1.,0.,0.));
#18500=DIRECTION('ref_axis',(0.,1.,0.));
#18501=DIRECTION('center_axis',(0.,-0.568064746731156,0.822983865893657));
#18502=DIRECTION('ref_axis',(0.,-0.822983865893656,-0.568064746731156));
#18503=DIRECTION('',(0.,-0.822983865893656,-0.568064746731156));
#18504=DIRECTION('',(1.,0.,0.));
#18505=DIRECTION('',(-0.707106781186546,-0.581937472380526,-0.401682434566619));
#18506=DIRECTION('',(0.,-0.822983865893656,-0.568064746731156));
#18507=DIRECTION('center_axis',(1.,0.,0.));
#18508=DIRECTION('ref_axis',(0.,-0.822983865893656,-0.568064746731156));
#18509=DIRECTION('',(0.,0.822983865893656,0.568064746731156));
#18510=DIRECTION('',(0.,0.568064746731156,-0.822983865893656));
#18511=DIRECTION('center_axis',(0.,0.568064746731156,-0.822983865893657));
#18512=DIRECTION('ref_axis',(0.,0.822983865893656,0.568064746731156));
#18513=DIRECTION('',(0.,0.822983865893656,0.568064746731156));
#18514=DIRECTION('',(0.707106781186546,0.581937472380526,0.401682434566619));
#18515=DIRECTION('',(1.,0.,0.));
#18516=DIRECTION('center_axis',(0.,0.828365800425665,-0.560187558488358));
#18517=DIRECTION('ref_axis',(-1.,0.,0.));
#18518=DIRECTION('',(-1.,0.,0.));
#18519=DIRECTION('',(1.,0.,0.));
#18520=DIRECTION('center_axis',(0.,0.670233338073619,0.742150437940108));
#18521=DIRECTION('ref_axis',(1.,0.,0.));
#18522=DIRECTION('',(-1.,0.,0.));
#18523=DIRECTION('',(1.,0.,0.));
#18524=DIRECTION('center_axis',(1.,0.,0.));
#18525=DIRECTION('ref_axis',(0.,1.,0.));
#18526=DIRECTION('center_axis',(-1.,0.,0.));
#18527=DIRECTION('ref_axis',(0.,1.,0.));
#18528=DIRECTION('center_axis',(1.,0.,0.));
#18529=DIRECTION('ref_axis',(0.,1.,0.));
#18530=DIRECTION('center_axis',(0.,-0.120536680255322,0.992708874098054));
#18531=DIRECTION('ref_axis',(0.,-0.992708874098054,-0.120536680255322));
#18532=DIRECTION('',(0.,-0.992708874098054,-0.120536680255322));
#18533=DIRECTION('',(1.,0.,0.));
#18534=DIRECTION('',(-0.707106781186546,-0.701951176618798,-0.0852323039902532));
#18535=DIRECTION('',(0.,-0.992708874098054,-0.120536680255322));
#18536=DIRECTION('center_axis',(1.,0.,0.));
#18537=DIRECTION('ref_axis',(0.,-0.992708874098054,-0.120536680255322));
#18538=DIRECTION('',(0.,0.992708874098054,0.120536680255322));
#18539=DIRECTION('',(0.,0.120536680255322,-0.992708874098054));
#18540=DIRECTION('center_axis',(0.,0.120536680255322,-0.992708874098054));
#18541=DIRECTION('ref_axis',(0.,0.992708874098054,0.120536680255322));
#18542=DIRECTION('',(0.,0.992708874098054,0.120536680255322));
#18543=DIRECTION('',(0.707106781186546,0.701951176618798,0.0852323039902532));
#18544=DIRECTION('',(1.,0.,0.));
#18545=DIRECTION('center_axis',(0.,0.473149350311789,-0.880982231545865));
#18546=DIRECTION('ref_axis',(-1.,0.,0.));
#18547=DIRECTION('',(-1.,0.,0.));
#18548=DIRECTION('',(1.,0.,0.));
#18549=DIRECTION('center_axis',(0.,0.938356653444149,0.345668614336183));
#18550=DIRECTION('ref_axis',(0.,-0.345668614336183,0.938356653444149));
#18551=DIRECTION('',(-1.,0.,0.));
#18552=DIRECTION('',(1.,0.,0.));
#18553=DIRECTION('center_axis',(1.,0.,0.));
#18554=DIRECTION('ref_axis',(0.,1.,0.));
#18555=DIRECTION('center_axis',(-1.,0.,0.));
#18556=DIRECTION('ref_axis',(0.,1.,0.));
#18557=DIRECTION('center_axis',(1.,0.,0.));
#18558=DIRECTION('ref_axis',(0.,1.,0.));
#18559=DIRECTION('center_axis',(0.,0.354604887042536,0.935016242685415));
#18560=DIRECTION('ref_axis',(0.,-0.935016242685415,0.354604887042536));
#18561=DIRECTION('',(0.,-0.935016242685415,0.354604887042536));
#18562=DIRECTION('',(1.,0.,0.));
#18563=DIRECTION('',(-0.707106781186546,-0.661156325722425,0.250743520269667));
#18564=DIRECTION('',(0.,-0.935016242685415,0.354604887042536));
#18565=DIRECTION('center_axis',(1.,0.,0.));
#18566=DIRECTION('ref_axis',(0.,-0.935016242685415,0.354604887042536));
#18567=DIRECTION('',(0.,0.935016242685415,-0.354604887042536));
#18568=DIRECTION('',(0.,-0.354604887042536,-0.935016242685415));
#18569=DIRECTION('center_axis',(0.,-0.354604887042536,-0.935016242685415));
#18570=DIRECTION('ref_axis',(0.,0.935016242685415,-0.354604887042536));
#18571=DIRECTION('',(0.,0.935016242685415,-0.354604887042536));
#18572=DIRECTION('',(0.707106781186546,0.661156325722425,-0.250743520269667));
#18573=DIRECTION('',(1.,0.,0.));
#18574=DIRECTION('center_axis',(0.,0.00954008610927885,-0.99995449234304));
#18575=DIRECTION('ref_axis',(-1.,0.,0.));
#18576=DIRECTION('',(-1.,0.,0.));
#18577=DIRECTION('',(1.,0.,0.));
#18578=DIRECTION('center_axis',(0.,0.991513767934188,-0.130001723053771));
#18579=DIRECTION('ref_axis',(0.,0.130001723053771,0.991513767934188));
#18580=DIRECTION('',(-1.,0.,0.));
#18581=DIRECTION('',(1.,0.,0.));
#18582=DIRECTION('center_axis',(1.,0.,0.));
#18583=DIRECTION('ref_axis',(0.,1.,0.));
#18584=DIRECTION('center_axis',(-1.,0.,0.));
#18585=DIRECTION('ref_axis',(0.,1.,0.));
#18586=DIRECTION('center_axis',(1.,0.,0.));
#18587=DIRECTION('ref_axis',(0.,1.,0.));
#18588=DIRECTION('center_axis',(0.,0.748510748171101,0.663122658240795));
#18589=DIRECTION('ref_axis',(0.,-0.663122658240795,0.748510748171101));
#18590=DIRECTION('',(0.,-0.663122658240795,0.748510748171101));
#18591=DIRECTION('',(1.,0.,0.));
#18592=DIRECTION('',(-0.707106781186547,-0.468898528400516,0.529277025822802));
#18593=DIRECTION('',(0.,-0.663122658240795,0.748510748171101));
#18594=DIRECTION('center_axis',(1.,0.,0.));
#18595=DIRECTION('ref_axis',(0.,-0.663122658240795,0.748510748171101));
#18596=DIRECTION('',(0.,0.663122658240795,-0.748510748171101));
#18597=DIRECTION('',(0.,-0.748510748171101,-0.663122658240795));
#18598=DIRECTION('center_axis',(0.,-0.748510748171101,-0.663122658240795));
#18599=DIRECTION('ref_axis',(0.,0.663122658240795,-0.748510748171101));
#18600=DIRECTION('',(0.,0.663122658240795,-0.748510748171101));
#18601=DIRECTION('',(0.707106781186547,0.468898528400516,-0.529277025822802));
#18602=DIRECTION('',(1.,0.,0.));
#18603=DIRECTION('center_axis',(0.,-0.456254696850359,-0.889849229702418));
#18604=DIRECTION('ref_axis',(-1.,0.,0.));
#18605=DIRECTION('',(1.,0.,0.));
#18606=DIRECTION('',(-1.,0.,0.));
#18607=DIRECTION('center_axis',(0.,0.970941817426052,0.239315664287557));
#18608=DIRECTION('ref_axis',(0.,-0.239315664287557,0.970941817426052));
#18609=DIRECTION('',(0.,-0.239315664287557,0.970941817426052));
#18610=DIRECTION('',(1.,0.,0.));
#18611=DIRECTION('',(-0.707106781186546,-0.169221729061895,0.686559543239553));
#18612=DIRECTION('',(0.,-0.239315664287557,0.970941817426052));
#18613=DIRECTION('center_axis',(0.,0.817527027226742,-0.575890232382705));
#18614=DIRECTION('ref_axis',(-1.,0.,0.));
#18615=DIRECTION('',(-1.,0.,0.));
#18616=DIRECTION('',(1.,0.,0.));
#18617=DIRECTION('center_axis',(1.,0.,0.));
#18618=DIRECTION('ref_axis',(0.,1.,0.));
#18619=DIRECTION('center_axis',(1.,0.,0.));
#18620=DIRECTION('ref_axis',(0.,1.,0.));
#18621=DIRECTION('center_axis',(-1.,0.,0.));
#18622=DIRECTION('ref_axis',(0.,1.,0.));
#18623=DIRECTION('center_axis',(0.,-0.970941817426052,-0.239315664287557));
#18624=DIRECTION('ref_axis',(0.,0.239315664287557,-0.970941817426052));
#18625=DIRECTION('',(0.,0.239315664287557,-0.970941817426052));
#18626=DIRECTION('',(0.707106781186546,0.169221729061895,-0.686559543239553));
#18627=DIRECTION('',(1.,0.,0.));
#18628=DIRECTION('',(0.,0.239315664287557,-0.970941817426052));
#18629=DIRECTION('center_axis',(1.,0.,0.));
#18630=DIRECTION('ref_axis',(0.,1.,0.));
#18631=DIRECTION('center_axis',(1.,0.,0.));
#18632=DIRECTION('ref_axis',(0.,0.,-1.));
#18633=DIRECTION('center_axis',(1.,0.,0.));
#18634=DIRECTION('ref_axis',(0.,0.,-1.));
#18635=DIRECTION('center_axis',(1.,0.,0.));
#18636=DIRECTION('ref_axis',(0.,1.,0.));
#18637=DIRECTION('center_axis',(1.,0.,0.));
#18638=DIRECTION('ref_axis',(0.,0.,-1.));
#18639=DIRECTION('',(-1.,0.,0.));
#18640=DIRECTION('center_axis',(-1.,0.,0.));
#18641=DIRECTION('ref_axis',(0.,-1.,0.));
#18642=DIRECTION('',(1.,0.,0.));
#18643=DIRECTION('center_axis',(1.,0.,0.));
#18644=DIRECTION('ref_axis',(0.,0.,-1.));
#18645=DIRECTION('',(-1.,0.,0.));
#18646=DIRECTION('center_axis',(-1.,0.,0.));
#18647=DIRECTION('ref_axis',(0.,-1.,0.));
#18648=DIRECTION('',(1.,0.,0.));
#18649=DIRECTION('center_axis',(1.,0.,0.));
#18650=DIRECTION('ref_axis',(0.,0.,-1.));
#18651=DIRECTION('',(-1.,0.,0.));
#18652=DIRECTION('center_axis',(-1.,0.,0.));
#18653=DIRECTION('ref_axis',(0.,-1.,0.));
#18654=DIRECTION('',(1.,0.,0.));
#18655=DIRECTION('center_axis',(1.,0.,0.));
#18656=DIRECTION('ref_axis',(0.,0.,-1.));
#18657=DIRECTION('',(-1.,0.,0.));
#18658=DIRECTION('center_axis',(-1.,0.,0.));
#18659=DIRECTION('ref_axis',(0.,-1.,0.));
#18660=DIRECTION('',(1.,0.,0.));
#18661=DIRECTION('center_axis',(1.,0.,0.));
#18662=DIRECTION('ref_axis',(0.,0.,-1.));
#18663=DIRECTION('center_axis',(1.,0.,0.));
#18664=DIRECTION('ref_axis',(0.,0.,-1.));
#18665=DIRECTION('center_axis',(1.,0.,0.));
#18666=DIRECTION('ref_axis',(0.,0.,-1.));
#18667=DIRECTION('center_axis',(1.,0.,0.));
#18668=DIRECTION('ref_axis',(0.,0.,-1.));
#18669=DIRECTION('center_axis',(1.,0.,0.));
#18670=DIRECTION('ref_axis',(0.,0.,-1.));
#18671=DIRECTION('',(-1.,0.,0.));
#18672=DIRECTION('center_axis',(-1.,0.,0.));
#18673=DIRECTION('ref_axis',(0.,1.,0.));
#18674=DIRECTION('',(1.,0.,0.));
#18675=DIRECTION('center_axis',(1.,0.,0.));
#18676=DIRECTION('ref_axis',(0.,0.,-1.));
#18677=DIRECTION('',(-1.,0.,0.));
#18678=DIRECTION('center_axis',(-1.,0.,0.));
#18679=DIRECTION('ref_axis',(0.,1.,0.));
#18680=DIRECTION('',(1.,0.,0.));
#18681=DIRECTION('center_axis',(1.,0.,0.));
#18682=DIRECTION('ref_axis',(0.,0.,-1.));
#18683=DIRECTION('',(-1.,0.,0.));
#18684=DIRECTION('center_axis',(-1.,0.,0.));
#18685=DIRECTION('ref_axis',(0.,-1.,0.));
#18686=DIRECTION('',(1.,0.,0.));
#18687=DIRECTION('center_axis',(1.,0.,0.));
#18688=DIRECTION('ref_axis',(0.,0.,-1.));
#18689=DIRECTION('',(-1.,0.,0.));
#18690=DIRECTION('center_axis',(-1.,0.,0.));
#18691=DIRECTION('ref_axis',(0.,-1.,0.));
#18692=DIRECTION('',(1.,0.,0.));
#18693=DIRECTION('center_axis',(1.,0.,0.));
#18694=DIRECTION('ref_axis',(0.,0.,-1.));
#18695=DIRECTION('',(-1.,0.,0.));
#18696=DIRECTION('center_axis',(-1.,0.,0.));
#18697=DIRECTION('ref_axis',(0.,-1.,0.));
#18698=DIRECTION('center_axis',(0.,-0.817527027226745,-0.575890232382701));
#18699=DIRECTION('ref_axis',(-1.,0.,0.));
#18700=DIRECTION('',(-1.,0.,0.));
#18701=DIRECTION('center_axis',(0.,0.456254696850359,-0.889849229702418));
#18702=DIRECTION('ref_axis',(-1.,0.,0.));
#18703=DIRECTION('',(1.,0.,0.));
#18704=DIRECTION('center_axis',(1.,0.,0.));
#18705=DIRECTION('ref_axis',(0.,-1.,0.));
#18706=DIRECTION('center_axis',(1.,0.,0.));
#18707=DIRECTION('ref_axis',(0.,-1.,0.));
#18708=DIRECTION('center_axis',(0.,0.970941817426052,-0.239315664287558));
#18709=DIRECTION('ref_axis',(0.,0.239315664287558,0.970941817426052));
#18710=DIRECTION('',(0.,0.239315664287558,0.970941817426052));
#18711=DIRECTION('',(1.,0.,0.));
#18712=DIRECTION('',(-0.707106781186545,0.169221729061896,0.686559543239555));
#18713=DIRECTION('',(0.,0.239315664287558,0.970941817426052));
#18714=DIRECTION('center_axis',(1.,0.,0.));
#18715=DIRECTION('ref_axis',(0.,0.239315664287558,0.970941817426052));
#18716=DIRECTION('',(0.,-0.239315664287558,-0.970941817426052));
#18717=DIRECTION('',(0.,-0.970941817426052,0.239315664287558));
#18718=DIRECTION('center_axis',(0.,-0.970941817426052,0.239315664287558));
#18719=DIRECTION('ref_axis',(0.,-0.239315664287558,-0.970941817426052));
#18720=DIRECTION('',(0.,-0.239315664287558,-0.970941817426052));
#18721=DIRECTION('',(0.707106781186545,-0.169221729061896,-0.686559543239555));
#18722=DIRECTION('',(1.,0.,0.));
#18723=DIRECTION('center_axis',(0.,-0.991513767934189,-0.130001723053764));
#18724=DIRECTION('ref_axis',(0.,0.130001723053764,-0.991513767934189));
#18725=DIRECTION('',(-1.,0.,0.));
#18726=DIRECTION('center_axis',(0.,-0.00954008610928227,-0.99995449234304));
#18727=DIRECTION('ref_axis',(-1.,0.,0.));
#18728=DIRECTION('',(1.,0.,0.));
#18729=DIRECTION('center_axis',(1.,0.,0.));
#18730=DIRECTION('ref_axis',(0.,-1.,0.));
#18731=DIRECTION('center_axis',(1.,0.,0.));
#18732=DIRECTION('ref_axis',(0.,-1.,0.));
#18733=DIRECTION('center_axis',(0.,0.748510748171101,-0.663122658240796));
#18734=DIRECTION('ref_axis',(0.,0.663122658240796,0.748510748171101));
#18735=DIRECTION('',(0.,0.663122658240796,0.748510748171101));
#18736=DIRECTION('',(1.,0.,0.));
#18737=DIRECTION('',(-0.707106781186547,0.468898528400516,0.529277025822802));
#18738=DIRECTION('',(0.,0.663122658240796,0.748510748171101));
#18739=DIRECTION('center_axis',(1.,0.,0.));
#18740=DIRECTION('ref_axis',(0.,0.663122658240796,0.748510748171101));
#18741=DIRECTION('',(0.,-0.663122658240796,-0.748510748171101));
#18742=DIRECTION('',(0.,-0.748510748171101,0.663122658240796));
#18743=DIRECTION('center_axis',(0.,-0.748510748171101,0.663122658240796));
#18744=DIRECTION('ref_axis',(0.,-0.663122658240796,-0.748510748171101));
#18745=DIRECTION('',(0.,-0.663122658240796,-0.748510748171101));
#18746=DIRECTION('',(0.707106781186547,-0.468898528400516,-0.529277025822802));
#18747=DIRECTION('',(1.,0.,0.));
#18748=DIRECTION('center_axis',(-0.707106781186549,0.,0.707106781186546));
#18749=DIRECTION('ref_axis',(0.707106781186546,0.,0.707106781186549));
#18750=DIRECTION('',(-0.707106781186546,0.,-0.707106781186549));
#18751=DIRECTION('',(0.,1.,0.));
#18752=DIRECTION('',(0.707106781186546,0.,0.707106781186549));
#18753=DIRECTION('',(0.,-1.,0.));
#18754=DIRECTION('center_axis',(0.,0.,-1.));
#18755=DIRECTION('ref_axis',(0.,1.,0.));
#18756=DIRECTION('',(1.,0.,0.));
#18757=DIRECTION('',(0.,1.,0.));
#18758=DIRECTION('',(1.,0.,0.));
#18759=DIRECTION('center_axis',(-0.707106781186548,-0.328608906326671,0.626111960181874));
#18760=DIRECTION('ref_axis',(0.662926885132466,0.,0.748684142324763));
#18761=DIRECTION('',(-0.707106781186547,0.328608906326672,-0.626111960181875));
#18762=DIRECTION('',(0.,0.88545602565321,0.464723172043769));
#18763=DIRECTION('',(0.707106781186547,-0.328608906326672,0.626111960181875));
#18764=DIRECTION('',(0.,-0.88545602565321,-0.464723172043769));
#18765=DIRECTION('center_axis',(0.,0.464723172043769,-0.88545602565321));
#18766=DIRECTION('ref_axis',(0.,0.88545602565321,0.464723172043769));
#18767=DIRECTION('',(1.,0.,0.));
#18768=DIRECTION('',(0.,0.88545602565321,0.464723172043769));
#18769=DIRECTION('',(1.,0.,0.));
#18770=DIRECTION('center_axis',(-0.707106781186548,-0.581937472380525,0.401682434566619));
#18771=DIRECTION('ref_axis',(0.493932454279441,0.,0.869500276371139));
#18772=DIRECTION('',(-0.707106781186547,0.581937472380525,-0.401682434566619));
#18773=DIRECTION('',(0.,0.568064746731156,0.822983865893656));
#18774=DIRECTION('',(0.707106781186547,-0.581937472380525,0.401682434566619));
#18775=DIRECTION('',(0.,-0.568064746731156,-0.822983865893656));
#18776=DIRECTION('center_axis',(0.,0.822983865893656,-0.568064746731156));
#18777=DIRECTION('ref_axis',(0.,0.568064746731156,0.822983865893656));
#18778=DIRECTION('',(1.,0.,0.));
#18779=DIRECTION('',(0.,0.568064746731156,0.822983865893656));
#18780=DIRECTION('',(1.,0.,0.));
#18781=DIRECTION('center_axis',(-0.707106781186548,-0.701951176618796,0.0852323039902536));
#18782=DIRECTION('ref_axis',(0.119670463698395,0.,0.992813668378015));
#18783=DIRECTION('',(-0.707106781186547,0.701951176618797,-0.0852323039902537));
#18784=DIRECTION('',(0.,0.120536680255323,0.992708874098054));
#18785=DIRECTION('',(0.707106781186547,-0.701951176618797,0.0852323039902537));
#18786=DIRECTION('',(0.,-0.120536680255323,-0.992708874098054));
#18787=DIRECTION('center_axis',(0.,0.992708874098054,-0.120536680255323));
#18788=DIRECTION('ref_axis',(0.,0.120536680255323,0.992708874098054));
#18789=DIRECTION('',(1.,0.,0.));
#18790=DIRECTION('',(0.,0.120536680255323,0.992708874098054));
#18791=DIRECTION('',(1.,0.,0.));
#18792=DIRECTION('center_axis',(-0.707106781186548,-0.661156325722423,-0.250743520269666));
#18793=DIRECTION('ref_axis',(-0.33421410555183,0.,0.942497178590042));
#18794=DIRECTION('',(-0.707106781186547,0.661156325722424,0.250743520269667));
#18795=DIRECTION('',(0.,-0.354604887042536,0.935016242685415));
#18796=DIRECTION('',(0.707106781186547,-0.661156325722424,-0.250743520269667));
#18797=DIRECTION('',(0.,0.354604887042536,-0.935016242685415));
#18798=DIRECTION('center_axis',(0.,0.935016242685415,0.354604887042536));
#18799=DIRECTION('ref_axis',(0.,-0.354604887042536,0.935016242685415));
#18800=DIRECTION('',(1.,0.,0.));
#18801=DIRECTION('',(0.,-0.354604887042536,0.935016242685415));
#18802=DIRECTION('',(1.,0.,0.));
#18803=DIRECTION('center_axis',(-0.707106781186548,-0.468898528400515,-0.529277025822801));
#18804=DIRECTION('ref_axis',(-0.59923668503494,0.,0.800571917636596));
#18805=DIRECTION('',(0.,-0.748510748171101,0.663122658240796));
#18806=DIRECTION('',(0.,0.748510748171101,-0.663122658240796));
#18807=DIRECTION('center_axis',(0.,0.663122658240796,0.748510748171101));
#18808=DIRECTION('ref_axis',(0.,-0.748510748171101,0.663122658240796));
#18809=DIRECTION('center_axis',(-0.70710678118655,-0.169221729061895,-0.686559543239549));
#18810=DIRECTION('ref_axis',(-0.696605990477037,0.,0.717453896798607));
#18811=DIRECTION('',(0.,-0.970941817426052,0.239315664287558));
#18812=DIRECTION('',(0.,0.970941817426052,-0.239315664287558));
#18813=DIRECTION('center_axis',(0.,0.239315664287558,0.970941817426052));
#18814=DIRECTION('ref_axis',(0.,-0.970941817426052,0.239315664287558));
#18815=DIRECTION('center_axis',(-0.707106781186549,0.169221729061895,-0.686559543239551));
#18816=DIRECTION('ref_axis',(-0.696605990477039,0.,0.717453896798605));
#18817=DIRECTION('',(0.,-0.970941817426052,-0.239315664287557));
#18818=DIRECTION('',(0.,0.970941817426052,0.239315664287557));
#18819=DIRECTION('center_axis',(0.,-0.239315664287557,0.970941817426052));
#18820=DIRECTION('ref_axis',(0.,-0.970941817426052,-0.239315664287557));
#18821=DIRECTION('',(0.,-0.970941817426052,-0.239315664287557));
#18822=DIRECTION('center_axis',(-0.707106781186548,0.468898528400515,-0.529277025822801));
#18823=DIRECTION('ref_axis',(-0.59923668503494,0.,0.800571917636595));
#18824=DIRECTION('',(0.,-0.748510748171101,-0.663122658240795));
#18825=DIRECTION('',(0.,0.748510748171101,0.663122658240795));
#18826=DIRECTION('center_axis',(0.,-0.663122658240795,0.748510748171101));
#18827=DIRECTION('ref_axis',(0.,-0.748510748171101,-0.663122658240795));
#18828=DIRECTION('center_axis',(-0.707106781186549,0.661156325722422,-0.250743520269666));
#18829=DIRECTION('ref_axis',(-0.334214105551829,0.,0.942497178590043));
#18830=DIRECTION('',(0.,-0.354604887042536,-0.935016242685415));
#18831=DIRECTION('',(0.,0.354604887042536,0.935016242685415));
#18832=DIRECTION('center_axis',(0.,-0.935016242685415,0.354604887042536));
#18833=DIRECTION('ref_axis',(0.,-0.354604887042536,-0.935016242685415));
#18834=DIRECTION('center_axis',(-0.707106781186549,0.701951176618796,0.0852323039902529));
#18835=DIRECTION('ref_axis',(0.119670463698394,0.,0.992813668378015));
#18836=DIRECTION('',(0.,0.120536680255322,-0.992708874098054));
#18837=DIRECTION('',(0.,-0.120536680255322,0.992708874098054));
#18838=DIRECTION('center_axis',(0.,-0.992708874098054,-0.120536680255322));
#18839=DIRECTION('ref_axis',(0.,0.120536680255322,-0.992708874098054));
#18840=DIRECTION('center_axis',(-0.707106781186549,0.581937472380524,0.401682434566618));
#18841=DIRECTION('ref_axis',(0.49393245427944,0.,0.86950027637114));
#18842=DIRECTION('',(0.,0.568064746731156,-0.822983865893656));
#18843=DIRECTION('',(0.,-0.568064746731156,0.822983865893656));
#18844=DIRECTION('center_axis',(0.,-0.822983865893657,-0.568064746731156));
#18845=DIRECTION('ref_axis',(0.,0.568064746731156,-0.822983865893656));
#18846=DIRECTION('center_axis',(0.,-0.938356653444149,0.345668614336183));
#18847=DIRECTION('ref_axis',(0.,-0.345668614336183,-0.938356653444149));
#18848=DIRECTION('',(-1.,0.,0.));
#18849=DIRECTION('center_axis',(0.,-0.473149350311788,-0.880982231545865));
#18850=DIRECTION('ref_axis',(-1.,0.,0.));
#18851=DIRECTION('',(1.,0.,0.));
#18852=DIRECTION('center_axis',(1.,0.,0.));
#18853=DIRECTION('ref_axis',(0.,-1.,0.));
#18854=DIRECTION('center_axis',(1.,0.,0.));
#18855=DIRECTION('ref_axis',(0.,-1.,0.));
#18856=DIRECTION('center_axis',(0.,0.354604887042536,-0.935016242685415));
#18857=DIRECTION('ref_axis',(0.,0.935016242685415,0.354604887042536));
#18858=DIRECTION('',(0.,0.935016242685415,0.354604887042536));
#18859=DIRECTION('',(0.,0.935016242685415,0.354604887042536));
#18860=DIRECTION('center_axis',(1.,0.,0.));
#18861=DIRECTION('ref_axis',(0.,0.935016242685415,0.354604887042536));
#18862=DIRECTION('',(0.,-0.935016242685415,-0.354604887042536));
#18863=DIRECTION('center_axis',(0.,-0.354604887042536,0.935016242685415));
#18864=DIRECTION('ref_axis',(0.,-0.935016242685415,-0.354604887042536));
#18865=DIRECTION('',(0.,-0.935016242685415,-0.354604887042536));
#18866=DIRECTION('center_axis',(0.,-0.670233338073617,0.742150437940109));
#18867=DIRECTION('ref_axis',(1.,0.,0.));
#18868=DIRECTION('',(-1.,0.,0.));
#18869=DIRECTION('center_axis',(0.,-0.828365800425666,-0.560187558488357));
#18870=DIRECTION('ref_axis',(-1.,0.,0.));
#18871=DIRECTION('',(1.,0.,0.));
#18872=DIRECTION('center_axis',(1.,0.,0.));
#18873=DIRECTION('ref_axis',(0.,-1.,0.));
#18874=DIRECTION('center_axis',(1.,0.,0.));
#18875=DIRECTION('ref_axis',(0.,-1.,0.));
#18876=DIRECTION('center_axis',(0.,-0.120536680255323,-0.992708874098054));
#18877=DIRECTION('ref_axis',(0.,0.992708874098054,-0.120536680255323));
#18878=DIRECTION('',(0.,0.992708874098054,-0.120536680255323));
#18879=DIRECTION('',(0.,0.992708874098054,-0.120536680255323));
#18880=DIRECTION('center_axis',(1.,0.,0.));
#18881=DIRECTION('ref_axis',(0.,0.992708874098054,-0.120536680255323));
#18882=DIRECTION('',(0.,-0.992708874098054,0.120536680255323));
#18883=DIRECTION('center_axis',(0.,0.120536680255323,0.992708874098054));
#18884=DIRECTION('ref_axis',(0.,-0.992708874098054,0.120536680255323));
#18885=DIRECTION('',(0.,-0.992708874098054,0.120536680255323));
#18886=DIRECTION('center_axis',(0.,-0.248567642137749,0.968614540094294));
#18887=DIRECTION('ref_axis',(1.,0.,0.));
#18888=DIRECTION('',(-1.,0.,0.));
#18889=DIRECTION('center_axis',(0.,-0.993813628552114,-0.111060666773083));
#18890=DIRECTION('ref_axis',(0.,0.111060666773083,-0.993813628552114));
#18891=DIRECTION('',(1.,0.,0.));
#18892=DIRECTION('center_axis',(1.,0.,0.));
#18893=DIRECTION('ref_axis',(0.,-1.,0.));
#18894=DIRECTION('center_axis',(1.,0.,0.));
#18895=DIRECTION('ref_axis',(0.,-1.,0.));
#18896=DIRECTION('center_axis',(0.,-0.568064746731156,-0.822983865893656));
#18897=DIRECTION('ref_axis',(0.,0.822983865893656,-0.568064746731156));
#18898=DIRECTION('',(0.,0.822983865893656,-0.568064746731156));
#18899=DIRECTION('',(0.,0.822983865893656,-0.568064746731156));
#18900=DIRECTION('center_axis',(1.,0.,0.));
#18901=DIRECTION('ref_axis',(0.,0.822983865893656,-0.568064746731156));
#18902=DIRECTION('',(0.,-0.822983865893656,0.568064746731156));
#18903=DIRECTION('center_axis',(0.,0.568064746731156,0.822983865893656));
#18904=DIRECTION('ref_axis',(0.,-0.822983865893656,0.568064746731156));
#18905=DIRECTION('',(0.,-0.822983865893656,0.568064746731156));
#18906=DIRECTION('center_axis',(0.,0.230041905047053,0.9731807241835));
#18907=DIRECTION('ref_axis',(1.,0.,0.));
#18908=DIRECTION('',(-1.,0.,0.));
#18909=DIRECTION('center_axis',(0.,-0.931590731129833,0.363508885273776));
#18910=DIRECTION('ref_axis',(0.,-0.363508885273776,-0.931590731129833));
#18911=DIRECTION('',(1.,0.,0.));
#18912=DIRECTION('center_axis',(1.,0.,0.));
#18913=DIRECTION('ref_axis',(0.,-1.,0.));
#18914=DIRECTION('center_axis',(1.,0.,0.));
#18915=DIRECTION('ref_axis',(0.,-1.,0.));
#18916=DIRECTION('center_axis',(0.,-0.88545602565321,-0.464723172043769));
#18917=DIRECTION('ref_axis',(0.,0.464723172043769,-0.88545602565321));
#18918=DIRECTION('',(0.,0.464723172043769,-0.88545602565321));
#18919=DIRECTION('',(0.,0.464723172043769,-0.88545602565321));
#18920=DIRECTION('center_axis',(1.,0.,0.));
#18921=DIRECTION('ref_axis',(0.,0.464723172043769,-0.88545602565321));
#18922=DIRECTION('',(0.,-0.464723172043769,0.88545602565321));
#18923=DIRECTION('center_axis',(0.,0.88545602565321,0.464723172043769));
#18924=DIRECTION('ref_axis',(0.,-0.464723172043769,0.88545602565321));
#18925=DIRECTION('',(0.,-0.464723172043769,0.88545602565321));
#18926=DIRECTION('center_axis',(0.,0.655951624091067,0.754802932461375));
#18927=DIRECTION('ref_axis',(1.,0.,0.));
#18928=DIRECTION('',(-1.,0.,0.));
#18929=DIRECTION('center_axis',(0.,-0.655951624091067,0.754802932461375));
#18930=DIRECTION('ref_axis',(1.,0.,0.));
#18931=DIRECTION('',(1.,0.,0.));
#18932=DIRECTION('center_axis',(1.,0.,0.));
#18933=DIRECTION('ref_axis',(0.,1.,0.));
#18934=DIRECTION('center_axis',(1.,0.,0.));
#18935=DIRECTION('ref_axis',(0.,1.,0.));
#18936=DIRECTION('center_axis',(1.,0.,0.));
#18937=DIRECTION('ref_axis',(0.,0.,-1.));
#18938=DIRECTION('',(0.,0.,1.));
#18939=DIRECTION('',(0.,0.,-1.));
#18940=DIRECTION('center_axis',(0.,1.,0.));
#18941=DIRECTION('ref_axis',(0.,0.,1.));
#18942=DIRECTION('',(0.,0.,1.));
#18943=DIRECTION('center_axis',(1.,0.,0.));
#18944=DIRECTION('ref_axis',(0.,1.,0.));
#18945=DIRECTION('center_axis',(1.,0.,0.));
#18946=DIRECTION('ref_axis',(0.,0.,-1.));
#18947=DIRECTION('center_axis',(-0.707106781186548,0.328608906326671,0.626111960181873));
#18948=DIRECTION('ref_axis',(0.662926885132466,0.,0.748684142324764));
#18949=DIRECTION('',(-0.707106781186547,-0.328608906326672,-0.626111960181875));
#18950=DIRECTION('',(0.,0.88545602565321,-0.464723172043769));
#18951=DIRECTION('',(0.707106781186547,0.328608906326672,0.626111960181875));
#18952=DIRECTION('',(0.,-0.88545602565321,0.464723172043769));
#18953=DIRECTION('center_axis',(0.,-0.464723172043769,-0.88545602565321));
#18954=DIRECTION('ref_axis',(0.,0.88545602565321,-0.464723172043769));
#18955=DIRECTION('',(1.,0.,0.));
#18956=DIRECTION('',(0.,0.88545602565321,-0.464723172043769));
#18957=DIRECTION('',(1.,0.,0.));
#18958=DIRECTION('center_axis',(0.,0.931590731129832,0.363508885273778));
#18959=DIRECTION('ref_axis',(0.,-0.363508885273778,0.931590731129832));
#18960=DIRECTION('',(-1.,0.,0.));
#18961=DIRECTION('center_axis',(0.,-0.230041905047054,0.9731807241835));
#18962=DIRECTION('ref_axis',(1.,0.,0.));
#18963=DIRECTION('',(1.,0.,0.));
#18964=DIRECTION('center_axis',(1.,0.,0.));
#18965=DIRECTION('ref_axis',(0.,1.,0.));
#18966=DIRECTION('center_axis',(1.,0.,0.));
#18967=DIRECTION('ref_axis',(0.,1.,0.));
#18968=DIRECTION('center_axis',(1.,0.,0.));
#18969=DIRECTION('ref_axis',(0.,-0.464723172043769,-0.88545602565321));
#18970=DIRECTION('',(0.,0.464723172043769,0.88545602565321));
#18971=DIRECTION('',(0.,-0.464723172043769,-0.88545602565321));
#18972=DIRECTION('center_axis',(0.,0.88545602565321,-0.464723172043769));
#18973=DIRECTION('ref_axis',(0.,0.464723172043769,0.88545602565321));
#18974=DIRECTION('',(0.,0.464723172043769,0.88545602565321));
#18975=DIRECTION('center_axis',(1.,0.,0.));
#18976=DIRECTION('ref_axis',(0.,1.,0.));
#18977=DIRECTION('center_axis',(1.,0.,0.));
#18978=DIRECTION('ref_axis',(0.,0.,-1.));
#18979=DIRECTION('center_axis',(-1.,0.,0.));
#18980=DIRECTION('ref_axis',(0.,0.,-1.));
#18981=DIRECTION('center_axis',(-1.,0.,0.));
#18982=DIRECTION('ref_axis',(0.,0.,-1.));
#18983=DIRECTION('',(0.707106781186546,-8.65956056235495E-17,-0.707106781186549));
#18984=DIRECTION('center_axis',(1.,0.,0.));
#18985=DIRECTION('ref_axis',(0.,0.,-1.));
#18986=DIRECTION('center_axis',(1.,0.,0.));
#18987=DIRECTION('ref_axis',(0.,0.,-1.));
#18988=DIRECTION('',(1.,0.,0.));
#18989=DIRECTION('center_axis',(1.,0.,0.));
#18990=DIRECTION('ref_axis',(0.,0.,-1.));
#18991=DIRECTION('center_axis',(-1.,0.,0.));
#18992=DIRECTION('ref_axis',(0.,0.,1.));
#18993=DIRECTION('',(0.,-0.464723172043769,-0.88545602565321));
#18994=DIRECTION('center_axis',(1.,0.,0.));
#18995=DIRECTION('ref_axis',(0.,0.,-1.));
#18996=DIRECTION('center_axis',(1.,0.,0.));
#18997=DIRECTION('ref_axis',(0.,0.,-1.));
#18998=DIRECTION('center_axis',(1.,0.,0.));
#18999=DIRECTION('ref_axis',(0.,0.,-1.));
#19000=DIRECTION('center_axis',(1.,0.,0.));
#19001=DIRECTION('ref_axis',(0.,0.,-1.));
#19002=DIRECTION('center_axis',(1.,0.,0.));
#19003=DIRECTION('ref_axis',(0.,0.,-1.));
#19004=DIRECTION('center_axis',(1.,0.,0.));
#19005=DIRECTION('ref_axis',(0.,0.,-1.));
#19006=DIRECTION('center_axis',(1.,0.,0.));
#19007=DIRECTION('ref_axis',(0.,0.,-1.));
#19008=DIRECTION('center_axis',(1.,0.,0.));
#19009=DIRECTION('ref_axis',(0.,0.,-1.));
#19010=DIRECTION('center_axis',(1.,0.,0.));
#19011=DIRECTION('ref_axis',(0.,0.,-1.));
#19012=DIRECTION('center_axis',(1.,0.,0.));
#19013=DIRECTION('ref_axis',(0.,0.,-1.));
#19014=DIRECTION('',(0.,0.,-1.));
#19015=DIRECTION('center_axis',(1.,0.,0.));
#19016=DIRECTION('ref_axis',(0.,0.,-1.));
#19017=DIRECTION('center_axis',(-1.,0.,0.));
#19018=DIRECTION('ref_axis',(0.,1.,0.));
#19019=DIRECTION('center_axis',(-1.,0.,0.));
#19020=DIRECTION('ref_axis',(0.,1.,0.));
#19021=DIRECTION('',(0.,0.,-1.));
#19022=DIRECTION('',(0.,1.,0.));
#19023=DIRECTION('',(0.,0.,-1.));
#19024=DIRECTION('center_axis',(0.,1.,0.));
#19025=DIRECTION('ref_axis',(1.,0.,0.));
#19026=DIRECTION('',(1.,0.,0.));
#19027=DIRECTION('',(1.,0.,0.));
#19028=DIRECTION('',(0.,0.,-1.));
#19029=DIRECTION('center_axis',(0.,-1.,0.));
#19030=DIRECTION('ref_axis',(-1.,0.,0.));
#19031=DIRECTION('',(-1.,0.,0.));
#19032=DIRECTION('',(0.,0.,-1.));
#19033=DIRECTION('',(-1.,0.,0.));
#19034=DIRECTION('center_axis',(1.,0.,0.));
#19035=DIRECTION('ref_axis',(0.,-1.,0.));
#19036=DIRECTION('center_axis',(1.,0.,0.));
#19037=DIRECTION('ref_axis',(0.,1.,0.));
#19038=DIRECTION('',(0.,-1.,0.));
#19039=DIRECTION('center_axis',(0.,0.,-1.));
#19040=DIRECTION('ref_axis',(-1.,0.,0.));
#19041=DIRECTION('center_axis',(0.,-0.88545602565321,0.464723172043769));
#19042=DIRECTION('ref_axis',(0.,-0.464723172043769,-0.88545602565321));
#19043=DIRECTION('center_axis',(1.,0.,0.));
#19044=DIRECTION('ref_axis',(0.,1.,0.));
#19045=DIRECTION('center_axis',(1.,0.,0.));
#19046=DIRECTION('ref_axis',(0.,1.,0.));
#19047=DIRECTION('center_axis',(1.,0.,0.));
#19048=DIRECTION('ref_axis',(0.,1.,0.));
#19049=DIRECTION('center_axis',(1.,0.,0.));
#19050=DIRECTION('ref_axis',(0.,1.,0.));
#19051=DIRECTION('center_axis',(1.,0.,0.));
#19052=DIRECTION('ref_axis',(0.,-0.239315664287557,0.970941817426052));
#19053=DIRECTION('center_axis',(1.,0.,0.));
#19054=DIRECTION('ref_axis',(0.,1.,0.));
#19055=DIRECTION('center_axis',(1.,0.,0.));
#19056=DIRECTION('ref_axis',(0.,1.,0.));
#19057=DIRECTION('center_axis',(1.,0.,0.));
#19058=DIRECTION('ref_axis',(0.,1.,0.));
#19059=DIRECTION('center_axis',(1.,0.,0.));
#19060=DIRECTION('ref_axis',(0.,1.,0.));
#19061=DIRECTION('center_axis',(1.,0.,0.));
#19062=DIRECTION('ref_axis',(0.,1.,0.));
#19063=DIRECTION('center_axis',(0.,-1.,0.));
#19064=DIRECTION('ref_axis',(0.,0.,-1.));
#19065=DIRECTION('center_axis',(1.,0.,0.));
#19066=DIRECTION('ref_axis',(0.,1.,0.));
#19067=DIRECTION('center_axis',(-1.,0.,0.));
#19068=DIRECTION('ref_axis',(0.,0.,1.));
#19069=DIRECTION('center_axis',(1.,0.,0.));
#19070=DIRECTION('ref_axis',(0.,0.,-1.));
#19071=DIRECTION('center_axis',(1.,0.,0.));
#19072=DIRECTION('ref_axis',(0.,1.,0.));
#19073=DIRECTION('center_axis',(1.,0.,0.));
#19074=DIRECTION('ref_axis',(0.,0.,-1.));
#19075=DIRECTION('',(-1.,0.,0.));
#19076=DIRECTION('center_axis',(1.,0.,0.));
#19077=DIRECTION('ref_axis',(0.,0.,-1.));
#19078=DIRECTION('center_axis',(1.,0.,0.));
#19079=DIRECTION('ref_axis',(0.,0.,-1.));
#19080=DIRECTION('center_axis',(1.,0.,0.));
#19081=DIRECTION('ref_axis',(0.,1.,0.));
#19082=DIRECTION('center_axis',(1.,0.,0.));
#19083=DIRECTION('ref_axis',(0.,0.,-1.));
#19084=DIRECTION('',(-1.,0.,0.));
#19085=DIRECTION('center_axis',(1.,0.,0.));
#19086=DIRECTION('ref_axis',(0.,0.,-1.));
#19087=DIRECTION('center_axis',(1.,0.,0.));
#19088=DIRECTION('ref_axis',(0.,0.,-1.));
#19089=DIRECTION('center_axis',(1.,0.,0.));
#19090=DIRECTION('ref_axis',(0.,1.,0.));
#19091=DIRECTION('center_axis',(1.,0.,0.));
#19092=DIRECTION('ref_axis',(0.,0.,-1.));
#19093=DIRECTION('',(-1.,0.,0.));
#19094=DIRECTION('center_axis',(-1.,0.,0.));
#19095=DIRECTION('ref_axis',(0.,1.,0.));
#19096=DIRECTION('center_axis',(1.,0.,0.));
#19097=DIRECTION('ref_axis',(0.,0.,-1.));
#19098=DIRECTION('',(-0.707106781186552,-0.707106781186543,-8.65956056235487E-17));
#19099=DIRECTION('center_axis',(1.,0.,0.));
#19100=DIRECTION('ref_axis',(0.,0.,-1.));
#19101=DIRECTION('axis',(0.,0.,1.));
#19102=DIRECTION('refdir',(1.,0.,0.));
#19103=DIRECTION('center_axis',(-0.707106781186546,0.,-0.707106781186549));
#19104=DIRECTION('ref_axis',(-0.707106781186549,0.,0.707106781186546));
#19105=DIRECTION('',(0.577350269189628,-0.577350269189625,-0.577350269189625));
#19106=DIRECTION('',(0.,-1.,0.));
#19107=DIRECTION('',(-0.577350269189628,-0.577350269189625,0.577350269189625));
#19108=DIRECTION('',(-0.577350269189627,0.577350269189627,0.577350269189624));
#19109=DIRECTION('',(0.,1.,0.));
#19110=DIRECTION('',(0.577350269189627,0.577350269189627,-0.577350269189624));
#19111=DIRECTION('center_axis',(0.,0.,-1.));
#19112=DIRECTION('ref_axis',(0.,1.,0.));
#19113=DIRECTION('',(-1.,0.,0.));
#19114=DIRECTION('',(0.,1.,0.));
#19115=DIRECTION('',(1.,0.,0.));
#19116=DIRECTION('center_axis',(0.,0.707106781186548,-0.707106781186548));
#19117=DIRECTION('ref_axis',(-1.,0.,0.));
#19118=DIRECTION('',(-0.577350269189626,-0.577350269189626,-0.577350269189626));
#19119=DIRECTION('',(1.,0.,0.));
#19120=DIRECTION('',(-0.577350269189611,0.577350269189633,0.577350269189633));
#19121=DIRECTION('',(0.577350269189611,0.577350269189633,0.577350269189633));
#19122=DIRECTION('center_axis',(-0.707106781186548,0.707106781186548,0.));
#19123=DIRECTION('ref_axis',(0.,0.,1.));
#19124=DIRECTION('',(0.,0.,1.));
#19125=DIRECTION('',(-0.577350269189626,-0.577350269189626,-0.577350269189626));
#19126=DIRECTION('',(0.577350269189626,0.577350269189626,-0.577350269189626));
#19127=DIRECTION('',(0.,0.,-1.));
#19128=DIRECTION('center_axis',(-0.707106781186548,0.,0.707106781186548));
#19129=DIRECTION('ref_axis',(0.707106781186548,0.,0.707106781186548));
#19130=DIRECTION('',(0.577350269189627,0.577350269189623,0.577350269189627));
#19131=DIRECTION('',(0.,1.,0.));
#19132=DIRECTION('',(-0.577350269189626,0.577350269189626,-0.577350269189626));
#19133=DIRECTION('',(0.,-1.,0.));
#19134=DIRECTION('',(0.577350269189626,-0.577350269189626,0.577350269189626));
#19135=DIRECTION('center_axis',(0.,0.,1.));
#19136=DIRECTION('ref_axis',(0.,-1.,0.));
#19137=DIRECTION('',(-1.,0.,0.));
#19138=DIRECTION('',(0.,-1.,0.));
#19139=DIRECTION('',(1.,0.,0.));
#19140=DIRECTION('center_axis',(0.,-0.70710678118655,0.707106781186545));
#19141=DIRECTION('ref_axis',(1.,0.,0.));
#19142=DIRECTION('',(-0.577350269189624,0.577350269189624,0.577350269189629));
#19143=DIRECTION('',(1.,0.,0.));
#19144=DIRECTION('',(-0.57735026918961,-0.577350269189632,-0.577350269189636));
#19145=DIRECTION('',(0.577350269189613,-0.57735026918963,-0.577350269189634));
#19146=DIRECTION('center_axis',(-0.707106781186548,-0.707106781186548,0.));
#19147=DIRECTION('ref_axis',(0.,0.,1.));
#19148=DIRECTION('',(0.577350269189626,-0.577350269189626,0.577350269189626));
#19149=DIRECTION('',(0.,0.,1.));
#19150=DIRECTION('',(0.,0.,-1.));
#19151=DIRECTION('center_axis',(0.,1.,0.));
#19152=DIRECTION('ref_axis',(0.,0.,1.));
#19153=DIRECTION('',(-1.,0.,0.));
#19154=DIRECTION('',(0.,0.,1.));
#19155=DIRECTION('center_axis',(0.707106781186561,0.,0.707106781186534));
#19156=DIRECTION('ref_axis',(0.707106781186534,0.,-0.707106781186561));
#19157=DIRECTION('',(0.577350269189611,0.577350269189633,-0.577350269189633));
#19158=DIRECTION('',(0.,1.,0.));
#19159=DIRECTION('',(-0.577350269189611,0.577350269189633,0.577350269189633));
#19160=DIRECTION('',(-0.577350269189611,-0.577350269189633,0.577350269189633));
#19161=DIRECTION('center_axis',(0.707106781186561,0.707106781186534,0.));
#19162=DIRECTION('ref_axis',(0.,0.,-1.));
#19163=DIRECTION('',(0.,0.,-1.));
#19164=DIRECTION('',(-0.577350269189611,0.577350269189633,-0.577350269189633));
#19165=DIRECTION('',(0.577350269189611,-0.577350269189633,0.577350269189633));
#19166=DIRECTION('center_axis',(1.,0.,0.));
#19167=DIRECTION('ref_axis',(0.,0.,-1.));
#19168=DIRECTION('',(0.,0.,1.));
#19169=DIRECTION('',(0.,-1.,0.));
#19170=DIRECTION('center_axis',(0.707106781186561,-0.707106781186534,0.));
#19171=DIRECTION('ref_axis',(0.,0.,-1.));
#19172=DIRECTION('',(0.,0.,-1.));
#19173=DIRECTION('',(0.577350269189611,0.577350269189633,-0.577350269189633));
#19174=DIRECTION('',(-0.577350269189611,-0.577350269189633,-0.577350269189633));
#19175=DIRECTION('center_axis',(0.707106781186561,0.,-0.707106781186534));
#19176=DIRECTION('ref_axis',(-0.707106781186534,0.,-0.707106781186561));
#19177=DIRECTION('',(-0.577350269189611,0.577350269189633,-0.577350269189633));
#19178=DIRECTION('center_axis',(0.,-0.707106781186548,-0.707106781186548));
#19179=DIRECTION('ref_axis',(-1.,0.,0.));
#19180=DIRECTION('',(-1.,0.,0.));
#19181=DIRECTION('center_axis',(0.,-1.,0.));
#19182=DIRECTION('ref_axis',(0.,0.,-1.));
#19183=DIRECTION('center_axis',(0.,0.707106781186548,0.707106781186548));
#19184=DIRECTION('ref_axis',(1.,0.,0.));
#19185=DIRECTION('center_axis',(1.,0.,0.));
#19186=DIRECTION('ref_axis',(0.,0.,-1.));
#19187=DIRECTION('axis',(0.,0.,1.));
#19188=DIRECTION('refdir',(1.,0.,0.));
#19189=DIRECTION('center_axis',(1.,0.,0.));
#19190=DIRECTION('ref_axis',(0.,1.,0.));
#19191=DIRECTION('center_axis',(1.,0.,0.));
#19192=DIRECTION('ref_axis',(0.,0.,-1.));
#19193=DIRECTION('',(-0.919145030018057,0.39391929857917,4.82412008127352E-17));
#19194=DIRECTION('center_axis',(1.,0.,0.));
#19195=DIRECTION('ref_axis',(0.,0.,-1.));
#19196=DIRECTION('center_axis',(-1.,0.,0.));
#19197=DIRECTION('ref_axis',(0.,0.,1.));
#19198=DIRECTION('center_axis',(1.,0.,0.));
#19199=DIRECTION('ref_axis',(0.,0.,-1.));
#19200=DIRECTION('center_axis',(-1.,0.,0.));
#19201=DIRECTION('ref_axis',(0.,1.,0.));
#19202=DIRECTION('',(-0.961523947640823,-0.274721127897378,-3.36436349937675E-17));
#19203=DIRECTION('center_axis',(1.,0.,0.));
#19204=DIRECTION('ref_axis',(0.,0.,-1.));
#19205=DIRECTION('center_axis',(-1.,0.,0.));
#19206=DIRECTION('ref_axis',(0.,0.,1.));
#19207=DIRECTION('center_axis',(1.,0.,0.));
#19208=DIRECTION('ref_axis',(0.,0.,-1.));
#19209=DIRECTION('center_axis',(1.,0.,0.));
#19210=DIRECTION('ref_axis',(0.,1.,0.));
#19211=DIRECTION('center_axis',(1.,0.,0.));
#19212=DIRECTION('ref_axis',(0.,0.,-1.));
#19213=DIRECTION('',(-0.707106781186547,0.707106781186548,8.65956056235494E-17));
#19214=DIRECTION('center_axis',(1.,0.,0.));
#19215=DIRECTION('ref_axis',(0.,1.,0.));
#19216=DIRECTION('center_axis',(1.,0.,0.));
#19217=DIRECTION('ref_axis',(0.,0.,-1.));
#19218=DIRECTION('',(-1.,0.,0.));
#19219=DIRECTION('center_axis',(-1.,0.,0.));
#19220=DIRECTION('ref_axis',(0.,1.,0.));
#19221=DIRECTION('center_axis',(1.,0.,0.));
#19222=DIRECTION('ref_axis',(0.,0.,-1.));
#19223=DIRECTION('',(-0.707106781186548,-0.707106781186548,-8.65956056235493E-17));
#19224=DIRECTION('center_axis',(1.,0.,0.));
#19225=DIRECTION('ref_axis',(0.,0.,-1.));
#19226=DIRECTION('center_axis',(1.,0.,0.));
#19227=DIRECTION('ref_axis',(0.,0.,-1.));
#19228=DIRECTION('center_axis',(1.,0.,0.));
#19229=DIRECTION('ref_axis',(0.,1.,0.));
#19230=DIRECTION('',(-0.961523947640823,0.274721127897378,3.36436349937675E-17));
#19231=DIRECTION('center_axis',(1.,0.,0.));
#19232=DIRECTION('ref_axis',(0.,0.,-1.));
#19233=DIRECTION('center_axis',(1.,0.,0.));
#19234=DIRECTION('ref_axis',(0.,0.,-1.));
#19235=DIRECTION('center_axis',(1.,0.,0.));
#19236=DIRECTION('ref_axis',(0.,0.,-1.));
#19237=DIRECTION('center_axis',(-1.,0.,0.));
#19238=DIRECTION('ref_axis',(0.,1.,0.));
#19239=DIRECTION('center_axis',(1.,0.,0.));
#19240=DIRECTION('ref_axis',(0.,0.,-1.));
#19241=DIRECTION('',(-0.919145030018057,-0.39391929857917,-4.82412008127351E-17));
#19242=DIRECTION('center_axis',(1.,0.,0.));
#19243=DIRECTION('ref_axis',(0.,0.,-1.));
#19244=DIRECTION('center_axis',(1.,0.,0.));
#19245=DIRECTION('ref_axis',(0.,0.,-1.));
#19246=DIRECTION('center_axis',(1.,0.,0.));
#19247=DIRECTION('ref_axis',(0.,1.,0.));
#19248=DIRECTION('',(-0.707106781186548,0.707106781186548,8.65956056235494E-17));
#19249=DIRECTION('center_axis',(1.,0.,0.));
#19250=DIRECTION('ref_axis',(0.,0.,-1.));
#19251=DIRECTION('center_axis',(1.,0.,0.));
#19252=DIRECTION('ref_axis',(0.,1.,0.));
#19253=DIRECTION('',(-1.,0.,0.));
#19254=DIRECTION('center_axis',(1.,0.,0.));
#19255=DIRECTION('ref_axis',(0.,0.,-1.));
#19256=DIRECTION('center_axis',(-1.,0.,0.));
#19257=DIRECTION('ref_axis',(0.,1.,0.));
#19258=DIRECTION('',(-0.707106781186547,-0.707106781186548,-8.65956056235494E-17));
#19259=DIRECTION('center_axis',(1.,0.,0.));
#19260=DIRECTION('ref_axis',(0.,0.,-1.));
#19261=DIRECTION('center_axis',(-1.,0.,0.));
#19262=DIRECTION('ref_axis',(0.,0.,1.));
#19263=DIRECTION('axis',(0.,0.,1.));
#19264=DIRECTION('refdir',(1.,0.,0.));
#19265=DIRECTION('center_axis',(1.,0.,0.));
#19266=DIRECTION('ref_axis',(0.,1.,0.));
#19267=DIRECTION('center_axis',(1.,0.,0.));
#19268=DIRECTION('ref_axis',(0.,0.,-1.));
#19269=DIRECTION('',(-1.,0.,0.));
#19270=DIRECTION('center_axis',(1.,0.,0.));
#19271=DIRECTION('ref_axis',(0.,0.,-1.));
#19272=DIRECTION('center_axis',(-1.,0.,0.));
#19273=DIRECTION('ref_axis',(0.,0.,1.));
#19274=DIRECTION('center_axis',(1.,0.,0.));
#19275=DIRECTION('ref_axis',(0.,1.,0.));
#19276=DIRECTION('center_axis',(1.,0.,0.));
#19277=DIRECTION('ref_axis',(0.,0.,-1.));
#19278=DIRECTION('center_axis',(-1.,0.,0.));
#19279=DIRECTION('ref_axis',(0.,1.,0.));
#19280=DIRECTION('center_axis',(1.,0.,0.));
#19281=DIRECTION('ref_axis',(0.,1.,0.));
#19282=DIRECTION('center_axis',(1.,0.,0.));
#19283=DIRECTION('ref_axis',(0.,0.,-1.));
#19284=DIRECTION('',(-1.,0.,0.));
#19285=DIRECTION('center_axis',(1.,0.,0.));
#19286=DIRECTION('ref_axis',(0.,1.,0.));
#19287=DIRECTION('center_axis',(1.,0.,0.));
#19288=DIRECTION('ref_axis',(0.,0.,-1.));
#19289=DIRECTION('',(-1.,0.,0.));
#19290=DIRECTION('center_axis',(1.,0.,0.));
#19291=DIRECTION('ref_axis',(0.,0.,-1.));
#19292=DIRECTION('center_axis',(-1.,0.,0.));
#19293=DIRECTION('ref_axis',(0.,0.,1.));
#19294=DIRECTION('center_axis',(1.,0.,0.));
#19295=DIRECTION('ref_axis',(0.,0.,-1.));
#19296=DIRECTION('center_axis',(1.,0.,0.));
#19297=DIRECTION('ref_axis',(0.,1.,0.));
#19298=DIRECTION('center_axis',(1.,0.,0.));
#19299=DIRECTION('ref_axis',(0.,0.,-1.));
#19300=DIRECTION('',(-1.,0.,0.));
#19301=DIRECTION('center_axis',(1.,0.,0.));
#19302=DIRECTION('ref_axis',(0.,0.,-1.));
#19303=DIRECTION('center_axis',(1.,0.,0.));
#19304=DIRECTION('ref_axis',(0.,0.,-1.));
#19305=DIRECTION('center_axis',(1.,0.,0.));
#19306=DIRECTION('ref_axis',(0.,1.,0.));
#19307=DIRECTION('',(-1.,0.,0.));
#19308=DIRECTION('center_axis',(1.,0.,0.));
#19309=DIRECTION('ref_axis',(0.,0.,-1.));
#19310=DIRECTION('center_axis',(-1.,0.,0.));
#19311=DIRECTION('ref_axis',(0.,0.,1.));
#19312=DIRECTION('center_axis',(1.,0.,0.));
#19313=DIRECTION('ref_axis',(0.,1.,0.));
#19314=DIRECTION('',(-1.,0.,0.));
#19315=DIRECTION('center_axis',(1.,0.,0.));
#19316=DIRECTION('ref_axis',(0.,0.,-1.));
#19317=DIRECTION('center_axis',(1.,0.,0.));
#19318=DIRECTION('ref_axis',(0.,0.,-1.));
#19319=DIRECTION('axis',(0.,0.,1.));
#19320=DIRECTION('refdir',(1.,0.,0.));
#19321=DIRECTION('center_axis',(1.,0.,0.));
#19322=DIRECTION('ref_axis',(0.,-1.,0.));
#19323=DIRECTION('center_axis',(-1.,0.,0.));
#19324=DIRECTION('ref_axis',(0.,-1.,0.));
#19325=DIRECTION('center_axis',(-1.,0.,0.));
#19326=DIRECTION('ref_axis',(0.,-1.,0.));
#19327=DIRECTION('',(0.707106781186547,0.707106781186547,-8.65956056235493E-17));
#19328=DIRECTION('center_axis',(1.,0.,0.));
#19329=DIRECTION('ref_axis',(0.,-1.,0.));
#19330=DIRECTION('center_axis',(1.,0.,0.));
#19331=DIRECTION('ref_axis',(0.,0.,-1.));
#19332=DIRECTION('center_axis',(1.,0.,0.));
#19333=DIRECTION('ref_axis',(0.,0.,-1.));
#19334=DIRECTION('center_axis',(1.,0.,0.));
#19335=DIRECTION('ref_axis',(0.,1.,0.));
#19336=DIRECTION('',(-1.,0.,0.));
#19337=DIRECTION('center_axis',(1.,0.,0.));
#19338=DIRECTION('ref_axis',(0.,0.,-1.));
#19339=DIRECTION('center_axis',(1.,0.,-6.79398744629287E-15));
#19340=DIRECTION('ref_axis',(0.,-1.,-3.10787303913223E-17));
#19341=DIRECTION('center_axis',(-1.,0.,0.));
#19342=DIRECTION('ref_axis',(0.,-1.,-6.12323399573677E-17));
#19343=DIRECTION('center_axis',(-1.,0.,0.));
#19344=DIRECTION('ref_axis',(0.,-1.,-6.12323399573677E-17));
#19345=DIRECTION('',(-0.289784148688431,-0.957092026489052,1.8218346946E-15));
#19346=DIRECTION('center_axis',(1.,0.,0.));
#19347=DIRECTION('ref_axis',(0.,-1.,0.));
#19348=DIRECTION('center_axis',(-1.,0.,0.));
#19349=DIRECTION('ref_axis',(0.,0.,1.));
#19350=DIRECTION('center_axis',(1.,0.,0.));
#19351=DIRECTION('ref_axis',(0.,0.,-1.));
#19352=DIRECTION('center_axis',(1.,0.,0.));
#19353=DIRECTION('ref_axis',(0.,1.,0.));
#19354=DIRECTION('center_axis',(1.,0.,0.));
#19355=DIRECTION('ref_axis',(0.,0.,-1.));
#19356=DIRECTION('',(-0.554700196225229,0.832050294337844,1.01896772969045E-16));
#19357=DIRECTION('center_axis',(1.,0.,0.));
#19358=DIRECTION('ref_axis',(0.,1.,0.));
#19359=DIRECTION('center_axis',(1.,0.,0.));
#19360=DIRECTION('ref_axis',(0.,0.,-1.));
#19361=DIRECTION('',(-1.,0.,0.));
#19362=DIRECTION('center_axis',(-1.,0.,0.));
#19363=DIRECTION('ref_axis',(0.,0.,1.));
#19364=DIRECTION('center_axis',(1.,0.,0.));
#19365=DIRECTION('ref_axis',(0.,0.,-1.));
#19366=DIRECTION('center_axis',(1.,0.,0.));
#19367=DIRECTION('ref_axis',(0.,1.,0.));
#19368=DIRECTION('',(-1.,0.,0.));
#19369=DIRECTION('center_axis',(1.,0.,0.));
#19370=DIRECTION('ref_axis',(0.,0.,-1.));
#19371=DIRECTION('center_axis',(1.,0.,0.));
#19372=DIRECTION('ref_axis',(0.,0.,-1.));
#19373=DIRECTION('center_axis',(1.,0.,0.));
#19374=DIRECTION('ref_axis',(0.,1.,0.));
#19375=DIRECTION('',(-0.554700196225229,0.832050294337844,1.01896772969045E-16));
#19376=DIRECTION('axis',(0.,0.,1.));
#19377=DIRECTION('refdir',(1.,0.,0.));
#19378=DIRECTION('center_axis',(1.,0.,0.));
#19379=DIRECTION('ref_axis',(0.,1.,0.));
#19380=DIRECTION('center_axis',(1.,0.,0.));
#19381=DIRECTION('ref_axis',(0.,1.,0.));
#19382=DIRECTION('',(-0.707106781186546,0.707106781186549,8.65956056235495E-17));
#19383=DIRECTION('center_axis',(-1.,0.,0.));
#19384=DIRECTION('ref_axis',(0.,1.,0.));
#19385=DIRECTION('center_axis',(1.,0.,0.));
#19386=DIRECTION('ref_axis',(0.,1.,0.));
#19387=DIRECTION('center_axis',(1.,0.,0.));
#19388=DIRECTION('ref_axis',(0.,0.,-1.));
#19389=DIRECTION('',(1.,0.,0.));
#19390=DIRECTION('center_axis',(1.,0.,0.));
#19391=DIRECTION('ref_axis',(0.,0.,-1.));
#19392=DIRECTION('center_axis',(1.,0.,0.));
#19393=DIRECTION('ref_axis',(0.,0.,-1.));
#19394=DIRECTION('center_axis',(1.,0.,0.));
#19395=DIRECTION('ref_axis',(0.,1.,0.));
#19396=DIRECTION('center_axis',(1.,0.,0.));
#19397=DIRECTION('ref_axis',(0.,1.,0.));
#19398=DIRECTION('',(1.,0.,0.));
#19399=DIRECTION('center_axis',(-1.,0.,0.));
#19400=DIRECTION('ref_axis',(0.,1.,0.));
#19401=DIRECTION('center_axis',(1.,0.,0.));
#19402=DIRECTION('ref_axis',(0.,1.,0.));
#19403=DIRECTION('center_axis',(-1.,0.,0.));
#19404=DIRECTION('ref_axis',(0.,0.,1.));
#19405=DIRECTION('center_axis',(1.,0.,0.));
#19406=DIRECTION('ref_axis',(0.,1.,0.));
#19407=DIRECTION('center_axis',(1.,0.,0.));
#19408=DIRECTION('ref_axis',(0.,0.,-1.));
#19409=DIRECTION('',(-1.,0.,0.));
#19410=DIRECTION('center_axis',(1.,0.,0.));
#19411=DIRECTION('ref_axis',(0.,0.,-1.));
#19412=DIRECTION('center_axis',(1.,0.,0.));
#19413=DIRECTION('ref_axis',(0.,0.,-1.));
#19414=DIRECTION('center_axis',(-1.,0.,0.));
#19415=DIRECTION('ref_axis',(0.,0.,1.));
#19416=DIRECTION('center_axis',(1.,0.,0.));
#19417=DIRECTION('ref_axis',(0.,0.,-1.));
#19418=DIRECTION('center_axis',(1.,0.,0.));
#19419=DIRECTION('ref_axis',(0.,1.,0.));
#19420=DIRECTION('center_axis',(1.,0.,0.));
#19421=DIRECTION('ref_axis',(0.,0.,-1.));
#19422=DIRECTION('',(-0.707106781186547,0.707106781186548,8.65956056235494E-17));
#19423=DIRECTION('center_axis',(1.,0.,0.));
#19424=DIRECTION('ref_axis',(0.,1.,0.));
#19425=DIRECTION('center_axis',(1.,0.,0.));
#19426=DIRECTION('ref_axis',(0.,0.,-1.));
#19427=DIRECTION('',(-1.,0.,0.));
#19428=DIRECTION('center_axis',(-1.,0.,0.));
#19429=DIRECTION('ref_axis',(0.,1.,0.));
#19430=DIRECTION('',(-0.707106781186547,-0.707106781186548,-8.65956056235494E-17));
#19431=DIRECTION('center_axis',(0.,-1.,-1.22464679914735E-16));
#19432=DIRECTION('ref_axis',(0.,-1.22464679914735E-16,1.));
#19433=DIRECTION('axis',(0.,0.,1.));
#19434=DIRECTION('refdir',(1.,0.,0.));
#19435=DIRECTION('center_axis',(1.,0.,0.));
#19436=DIRECTION('ref_axis',(0.,1.,0.));
#19437=DIRECTION('center_axis',(1.,0.,0.));
#19438=DIRECTION('ref_axis',(0.,0.,-1.));
#19439=DIRECTION('',(-1.,0.,0.));
#19440=DIRECTION('center_axis',(1.,0.,0.));
#19441=DIRECTION('ref_axis',(0.,0.,-1.));
#19442=DIRECTION('center_axis',(-1.,0.,0.));
#19443=DIRECTION('ref_axis',(0.,0.,1.));
#19444=DIRECTION('center_axis',(1.,0.,0.));
#19445=DIRECTION('ref_axis',(0.,0.,-1.));
#19446=DIRECTION('center_axis',(1.,0.,0.));
#19447=DIRECTION('ref_axis',(0.,1.,0.));
#19448=DIRECTION('center_axis',(1.,0.,0.));
#19449=DIRECTION('ref_axis',(0.,0.,-1.));
#19450=DIRECTION('',(-0.707106781186547,0.707106781186548,8.65956056235494E-17));
#19451=DIRECTION('center_axis',(1.,0.,0.));
#19452=DIRECTION('ref_axis',(0.,1.,0.));
#19453=DIRECTION('center_axis',(1.,0.,0.));
#19454=DIRECTION('ref_axis',(0.,0.,-1.));
#19455=DIRECTION('',(-1.,0.,0.));
#19456=DIRECTION('center_axis',(1.,0.,0.));
#19457=DIRECTION('ref_axis',(0.,0.,-1.));
#19458=DIRECTION('center_axis',(1.,0.,0.));
#19459=DIRECTION('ref_axis',(0.,0.,-1.));
#19460=DIRECTION('center_axis',(1.,0.,0.));
#19461=DIRECTION('ref_axis',(0.,1.,0.));
#19462=DIRECTION('center_axis',(1.,0.,0.));
#19463=DIRECTION('ref_axis',(0.,0.,-1.));
#19464=DIRECTION('',(-1.,0.,0.));
#19465=DIRECTION('center_axis',(1.,0.,0.));
#19466=DIRECTION('ref_axis',(0.,0.,-1.));
#19467=DIRECTION('center_axis',(1.,0.,0.));
#19468=DIRECTION('ref_axis',(0.,0.,-1.));
#19469=DIRECTION('center_axis',(0.,0.,1.));
#19470=DIRECTION('ref_axis',(1.,0.,0.));
#19471=DIRECTION('center_axis',(1.,0.,0.));
#19472=DIRECTION('ref_axis',(0.,0.,-1.));
#19473=DIRECTION('center_axis',(1.22464679914735E-16,-1.,0.));
#19474=DIRECTION('ref_axis',(-1.,-1.22464679914735E-16,0.));
#19475=DIRECTION('center_axis',(1.,0.,0.));
#19476=DIRECTION('ref_axis',(0.,0.,-1.));
#19477=DIRECTION('center_axis',(1.,0.,0.));
#19478=DIRECTION('ref_axis',(0.,0.,-1.));
#19479=DIRECTION('center_axis',(1.22464679914735E-16,-1.,0.));
#19480=DIRECTION('ref_axis',(-1.,-1.22464679914735E-16,0.));
#19481=DIRECTION('center_axis',(1.,0.,0.));
#19482=DIRECTION('ref_axis',(0.,1.,0.));
#19483=DIRECTION('',(-1.,0.,0.));
#19484=DIRECTION('center_axis',(1.,0.,0.));
#19485=DIRECTION('ref_axis',(0.,0.,-1.));
#19486=DIRECTION('center_axis',(-1.,0.,0.));
#19487=DIRECTION('ref_axis',(0.,0.,1.));
#19488=DIRECTION('axis',(0.,0.,1.));
#19489=DIRECTION('refdir',(1.,0.,0.));
#19490=DIRECTION('center_axis',(-1.,0.,0.));
#19491=DIRECTION('ref_axis',(0.,-1.,0.));
#19492=DIRECTION('center_axis',(-1.,0.,0.));
#19493=DIRECTION('ref_axis',(0.,-1.,0.));
#19494=DIRECTION('',(-0.707106781186555,0.70710678118654,8.65956056235484E-17));
#19495=DIRECTION('center_axis',(1.,0.,0.));
#19496=DIRECTION('ref_axis',(0.,-1.,0.));
#19497=DIRECTION('center_axis',(1.,0.,0.));
#19498=DIRECTION('ref_axis',(0.,-1.,0.));
#19499=DIRECTION('center_axis',(1.,0.,0.));
#19500=DIRECTION('ref_axis',(0.,0.,-1.));
#19501=DIRECTION('center_axis',(-1.,0.,0.));
#19502=DIRECTION('ref_axis',(0.,-0.78183148246803,-0.623489801858733));
#19503=DIRECTION('center_axis',(1.,0.,0.));
#19504=DIRECTION('ref_axis',(0.,0.,-1.));
#19505=DIRECTION('center_axis',(-1.,0.,0.));
#19506=DIRECTION('ref_axis',(0.,-0.974927912181824,0.222520933956315));
#19507=DIRECTION('center_axis',(1.,0.,0.));
#19508=DIRECTION('ref_axis',(0.,0.,-1.));
#19509=DIRECTION('center_axis',(-1.,0.,0.));
#19510=DIRECTION('ref_axis',(0.,-0.433883739117558,0.900968867902419));
#19511=DIRECTION('center_axis',(1.,0.,0.));
#19512=DIRECTION('ref_axis',(0.,0.,-1.));
#19513=DIRECTION('center_axis',(-1.,0.,0.));
#19514=DIRECTION('ref_axis',(0.,0.433883739117558,0.900968867902419));
#19515=DIRECTION('center_axis',(1.,0.,0.));
#19516=DIRECTION('ref_axis',(0.,0.,-1.));
#19517=DIRECTION('center_axis',(-1.,0.,0.));
#19518=DIRECTION('ref_axis',(0.,0.974927912181824,0.222520933956314));
#19519=DIRECTION('center_axis',(1.,0.,0.));
#19520=DIRECTION('ref_axis',(0.,0.,-1.));
#19521=DIRECTION('center_axis',(-1.,0.,0.));
#19522=DIRECTION('ref_axis',(0.,0.78183148246803,-0.623489801858734));
#19523=DIRECTION('center_axis',(1.,0.,0.));
#19524=DIRECTION('ref_axis',(0.,0.,-1.));
#19525=DIRECTION('center_axis',(-1.,0.,0.));
#19526=DIRECTION('ref_axis',(0.,0.,-1.));
#19527=DIRECTION('center_axis',(1.,0.,0.));
#19528=DIRECTION('ref_axis',(0.,0.,-1.));
#19529=DIRECTION('center_axis',(1.,0.,0.));
#19530=DIRECTION('ref_axis',(0.,1.,0.));
#19531=DIRECTION('',(-1.,0.,0.));
#19532=DIRECTION('center_axis',(1.,0.,0.));
#19533=DIRECTION('ref_axis',(0.,0.,-1.));
#19534=DIRECTION('center_axis',(1.,0.,0.));
#19535=DIRECTION('ref_axis',(0.,0.78183148246803,0.623489801858733));
#19536=DIRECTION('center_axis',(1.,0.,0.));
#19537=DIRECTION('ref_axis',(0.,-0.78183148246803,-0.623489801858733));
#19538=DIRECTION('',(-1.,0.,0.));
#19539=DIRECTION('',(1.,0.,0.));
#19540=DIRECTION('center_axis',(1.,0.,0.));
#19541=DIRECTION('ref_axis',(0.,1.,0.));
#19542=DIRECTION('center_axis',(1.,0.,0.));
#19543=DIRECTION('ref_axis',(0.,0.,-1.));
#19544=DIRECTION('',(1.,0.,0.));
#19545=DIRECTION('center_axis',(1.,0.,0.));
#19546=DIRECTION('ref_axis',(0.,0.974927912181824,-0.222520933956315));
#19547=DIRECTION('center_axis',(1.,0.,0.));
#19548=DIRECTION('ref_axis',(0.,-0.974927912181824,0.222520933956315));
#19549=DIRECTION('',(-1.,0.,0.));
#19550=DIRECTION('center_axis',(1.,0.,0.));
#19551=DIRECTION('ref_axis',(0.,1.,0.));
#19552=DIRECTION('center_axis',(1.,0.,0.));
#19553=DIRECTION('ref_axis',(0.,0.,-1.));
#19554=DIRECTION('',(1.,0.,0.));
#19555=DIRECTION('center_axis',(1.,0.,0.));
#19556=DIRECTION('ref_axis',(0.,0.433883739117558,-0.900968867902419));
#19557=DIRECTION('center_axis',(1.,0.,0.));
#19558=DIRECTION('ref_axis',(0.,-0.433883739117558,0.900968867902419));
#19559=DIRECTION('',(-1.,0.,0.));
#19560=DIRECTION('center_axis',(1.,0.,0.));
#19561=DIRECTION('ref_axis',(0.,1.,0.));
#19562=DIRECTION('center_axis',(1.,0.,0.));
#19563=DIRECTION('ref_axis',(0.,0.,-1.));
#19564=DIRECTION('',(1.,0.,0.));
#19565=DIRECTION('center_axis',(1.,0.,0.));
#19566=DIRECTION('ref_axis',(0.,-0.433883739117558,-0.900968867902419));
#19567=DIRECTION('center_axis',(1.,0.,0.));
#19568=DIRECTION('ref_axis',(0.,0.433883739117558,0.900968867902419));
#19569=DIRECTION('',(-1.,0.,0.));
#19570=DIRECTION('center_axis',(1.,0.,0.));
#19571=DIRECTION('ref_axis',(0.,1.,0.));
#19572=DIRECTION('center_axis',(1.,0.,0.));
#19573=DIRECTION('ref_axis',(0.,0.,-1.));
#19574=DIRECTION('',(1.,0.,0.));
#19575=DIRECTION('center_axis',(1.,0.,0.));
#19576=DIRECTION('ref_axis',(0.,-0.974927912181824,-0.222520933956314));
#19577=DIRECTION('center_axis',(1.,0.,0.));
#19578=DIRECTION('ref_axis',(0.,0.974927912181824,0.222520933956314));
#19579=DIRECTION('',(-1.,0.,0.));
#19580=DIRECTION('center_axis',(1.,0.,0.));
#19581=DIRECTION('ref_axis',(0.,1.,0.));
#19582=DIRECTION('center_axis',(1.,0.,0.));
#19583=DIRECTION('ref_axis',(0.,0.,-1.));
#19584=DIRECTION('',(1.,0.,0.));
#19585=DIRECTION('center_axis',(1.,0.,0.));
#19586=DIRECTION('ref_axis',(0.,-0.78183148246803,0.623489801858734));
#19587=DIRECTION('center_axis',(1.,0.,0.));
#19588=DIRECTION('ref_axis',(0.,0.78183148246803,-0.623489801858734));
#19589=DIRECTION('',(-1.,0.,0.));
#19590=DIRECTION('center_axis',(1.,0.,0.));
#19591=DIRECTION('ref_axis',(0.,1.,0.));
#19592=DIRECTION('center_axis',(1.,0.,0.));
#19593=DIRECTION('ref_axis',(0.,0.,-1.));
#19594=DIRECTION('',(1.,0.,0.));
#19595=DIRECTION('center_axis',(1.,0.,0.));
#19596=DIRECTION('ref_axis',(0.,-1.22464679914735E-16,1.));
#19597=DIRECTION('center_axis',(1.,0.,0.));
#19598=DIRECTION('ref_axis',(0.,0.,-1.));
#19599=DIRECTION('',(-1.,0.,0.));
#19600=DIRECTION('center_axis',(-1.,0.,0.));
#19601=DIRECTION('ref_axis',(0.,0.,1.));
#19602=DIRECTION('center_axis',(1.,0.,0.));
#19603=DIRECTION('ref_axis',(0.,0.,-1.));
#19604=DIRECTION('center_axis',(1.,0.,0.));
#19605=DIRECTION('ref_axis',(0.,0.,-1.));
#19606=DIRECTION('center_axis',(1.,0.,0.));
#19607=DIRECTION('ref_axis',(0.,1.,0.));
#19608=DIRECTION('center_axis',(1.,0.,0.));
#19609=DIRECTION('ref_axis',(0.,1.,0.));
#19610=DIRECTION('',(-0.707106781186549,0.707106781186546,8.65956056235492E-17));
#19611=DIRECTION('axis',(0.,0.,1.));
#19612=DIRECTION('refdir',(1.,0.,0.));
#19613=DIRECTION('center_axis',(1.,0.,0.));
#19614=DIRECTION('ref_axis',(0.,1.,0.));
#19615=DIRECTION('',(-1.,0.,0.));
#19616=DIRECTION('center_axis',(1.,0.,0.));
#19617=DIRECTION('ref_axis',(0.,1.,0.));
#19618=DIRECTION('center_axis',(1.,0.,0.));
#19619=DIRECTION('ref_axis',(0.,1.,0.));
#19620=DIRECTION('',(-1.,0.,0.));
#19621=DIRECTION('center_axis',(1.,0.,0.));
#19622=DIRECTION('ref_axis',(0.,1.,0.));
#19623=DIRECTION('',(-1.,0.,0.));
#19624=DIRECTION('center_axis',(1.,0.,0.));
#19625=DIRECTION('ref_axis',(0.,1.,0.));
#19626=DIRECTION('',(-1.,0.,0.));
#19627=DIRECTION('center_axis',(1.,0.,0.));
#19628=DIRECTION('ref_axis',(0.,1.,0.));
#19629=DIRECTION('',(-1.,0.,0.));
#19630=DIRECTION('center_axis',(1.,0.,0.));
#19631=DIRECTION('ref_axis',(0.,1.,0.));
#19632=DIRECTION('',(-1.,0.,0.));
#19633=DIRECTION('center_axis',(1.,0.,0.));
#19634=DIRECTION('ref_axis',(0.,1.,0.));
#19635=DIRECTION('',(-1.,0.,0.));
#19636=DIRECTION('center_axis',(1.,0.,0.));
#19637=DIRECTION('ref_axis',(0.,1.,0.));
#19638=DIRECTION('',(-1.,0.,0.));
#19639=DIRECTION('center_axis',(1.,0.,0.));
#19640=DIRECTION('ref_axis',(0.,1.,0.));
#19641=DIRECTION('',(-1.,0.,0.));
#19642=DIRECTION('center_axis',(1.,0.,0.));
#19643=DIRECTION('ref_axis',(0.,1.,0.));
#19644=DIRECTION('',(-1.,0.,0.));
#19645=DIRECTION('center_axis',(1.,0.,0.));
#19646=DIRECTION('ref_axis',(0.,1.,0.));
#19647=DIRECTION('',(-1.,0.,0.));
#19648=DIRECTION('center_axis',(1.,0.,0.));
#19649=DIRECTION('ref_axis',(0.,1.,0.));
#19650=DIRECTION('',(-1.,0.,0.));
#19651=DIRECTION('center_axis',(1.,0.,0.));
#19652=DIRECTION('ref_axis',(0.,1.,0.));
#19653=DIRECTION('',(-1.,0.,0.));
#19654=DIRECTION('center_axis',(1.,0.,0.));
#19655=DIRECTION('ref_axis',(0.,1.,0.));
#19656=DIRECTION('',(-1.,0.,0.));
#19657=DIRECTION('center_axis',(1.,0.,0.));
#19658=DIRECTION('ref_axis',(0.,1.,0.));
#19659=DIRECTION('',(-1.,0.,0.));
#19660=DIRECTION('center_axis',(1.,0.,0.));
#19661=DIRECTION('ref_axis',(0.,1.,0.));
#19662=DIRECTION('',(-1.,0.,0.));
#19663=DIRECTION('center_axis',(1.,0.,0.));
#19664=DIRECTION('ref_axis',(0.,1.,0.));
#19665=DIRECTION('',(-1.,0.,0.));
#19666=DIRECTION('center_axis',(1.,0.,0.));
#19667=DIRECTION('ref_axis',(0.,1.,0.));
#19668=DIRECTION('',(-1.,0.,0.));
#19669=DIRECTION('center_axis',(1.,0.,0.));
#19670=DIRECTION('ref_axis',(0.,1.,0.));
#19671=DIRECTION('',(-1.,0.,0.));
#19672=DIRECTION('center_axis',(1.,0.,0.));
#19673=DIRECTION('ref_axis',(0.,1.,0.));
#19674=DIRECTION('',(-1.,0.,0.));
#19675=DIRECTION('center_axis',(1.,0.,0.));
#19676=DIRECTION('ref_axis',(0.,1.,0.));
#19677=DIRECTION('',(-1.,0.,0.));
#19678=DIRECTION('center_axis',(1.,0.,0.));
#19679=DIRECTION('ref_axis',(0.,1.,0.));
#19680=DIRECTION('',(-1.,0.,0.));
#19681=DIRECTION('center_axis',(1.,0.,0.));
#19682=DIRECTION('ref_axis',(0.,1.,0.));
#19683=DIRECTION('',(-1.,0.,0.));
#19684=DIRECTION('center_axis',(1.,0.,0.));
#19685=DIRECTION('ref_axis',(0.,1.,0.));
#19686=DIRECTION('',(-1.,0.,0.));
#19687=DIRECTION('center_axis',(1.,0.,0.));
#19688=DIRECTION('ref_axis',(0.,1.,0.));
#19689=DIRECTION('',(-1.,0.,0.));
#19690=DIRECTION('center_axis',(1.,0.,0.));
#19691=DIRECTION('ref_axis',(0.,1.,0.));
#19692=DIRECTION('',(-1.,0.,0.));
#19693=DIRECTION('center_axis',(1.,0.,0.));
#19694=DIRECTION('ref_axis',(0.,1.,0.));
#19695=DIRECTION('',(-1.,0.,0.));
#19696=DIRECTION('center_axis',(1.,0.,0.));
#19697=DIRECTION('ref_axis',(0.,1.,0.));
#19698=DIRECTION('',(-1.,0.,0.));
#19699=DIRECTION('center_axis',(1.,0.,0.));
#19700=DIRECTION('ref_axis',(0.,1.,0.));
#19701=DIRECTION('',(-1.,0.,0.));
#19702=DIRECTION('center_axis',(1.,0.,0.));
#19703=DIRECTION('ref_axis',(0.,1.,0.));
#19704=DIRECTION('',(-1.,0.,0.));
#19705=DIRECTION('center_axis',(1.,0.,0.));
#19706=DIRECTION('ref_axis',(0.,1.,0.));
#19707=DIRECTION('',(-1.,0.,0.));
#19708=DIRECTION('center_axis',(1.,0.,0.));
#19709=DIRECTION('ref_axis',(0.,1.,0.));
#19710=DIRECTION('',(-1.,0.,0.));
#19711=DIRECTION('center_axis',(1.,0.,0.));
#19712=DIRECTION('ref_axis',(0.,1.,0.));
#19713=DIRECTION('',(-1.,0.,0.));
#19714=DIRECTION('center_axis',(1.,0.,0.));
#19715=DIRECTION('ref_axis',(0.,1.,0.));
#19716=DIRECTION('',(-1.,0.,0.));
#19717=DIRECTION('center_axis',(1.,0.,0.));
#19718=DIRECTION('ref_axis',(0.,-0.320272933918672,-0.947325312550618));
#19719=DIRECTION('',(1.,0.,0.));
#19720=DIRECTION('center_axis',(1.,0.,0.));
#19721=DIRECTION('ref_axis',(0.,1.,-2.86062230339267E-13));
#19722=DIRECTION('center_axis',(1.,0.,0.));
#19723=DIRECTION('ref_axis',(0.,1.,-2.86062230339267E-13));
#19724=DIRECTION('',(1.,0.,0.));
#19725=DIRECTION('center_axis',(1.,0.,0.));
#19726=DIRECTION('ref_axis',(0.,1.,-2.86062230339267E-13));
#19727=DIRECTION('',(1.,0.,0.));
#19728=DIRECTION('center_axis',(1.,0.,0.));
#19729=DIRECTION('ref_axis',(0.,1.,-2.86062230339267E-13));
#19730=DIRECTION('',(1.,0.,0.));
#19731=DIRECTION('center_axis',(1.,0.,0.));
#19732=DIRECTION('ref_axis',(0.,1.,-2.86062230339267E-13));
#19733=DIRECTION('',(1.,0.,0.));
#19734=DIRECTION('center_axis',(1.,0.,0.));
#19735=DIRECTION('ref_axis',(0.,1.,-2.86062230339267E-13));
#19736=DIRECTION('',(1.,0.,0.));
#19737=DIRECTION('center_axis',(1.,0.,0.));
#19738=DIRECTION('ref_axis',(0.,1.,-2.86062230339267E-13));
#19739=DIRECTION('',(1.,0.,0.));
#19740=DIRECTION('center_axis',(1.,0.,0.));
#19741=DIRECTION('ref_axis',(0.,1.,-2.86062230339267E-13));
#19742=DIRECTION('',(1.,0.,0.));
#19743=DIRECTION('center_axis',(1.,0.,0.));
#19744=DIRECTION('ref_axis',(0.,1.,-2.86062230339267E-13));
#19745=DIRECTION('',(1.,0.,0.));
#19746=DIRECTION('center_axis',(1.,0.,0.));
#19747=DIRECTION('ref_axis',(0.,1.,-2.86062230339267E-13));
#19748=DIRECTION('',(1.,0.,0.));
#19749=DIRECTION('center_axis',(1.,0.,0.));
#19750=DIRECTION('ref_axis',(0.,1.,-2.86062230339267E-13));
#19751=DIRECTION('',(1.,0.,0.));
#19752=DIRECTION('center_axis',(1.,0.,0.));
#19753=DIRECTION('ref_axis',(0.,1.,-2.86062230339267E-13));
#19754=DIRECTION('',(1.,0.,0.));
#19755=DIRECTION('center_axis',(1.,0.,0.));
#19756=DIRECTION('ref_axis',(0.,1.,-2.86062230339267E-13));
#19757=DIRECTION('',(1.,0.,0.));
#19758=DIRECTION('center_axis',(1.,0.,0.));
#19759=DIRECTION('ref_axis',(0.,1.,-2.86062230339267E-13));
#19760=DIRECTION('',(1.,0.,0.));
#19761=DIRECTION('center_axis',(1.,0.,0.));
#19762=DIRECTION('ref_axis',(0.,1.,-2.86062230339267E-13));
#19763=DIRECTION('',(1.,0.,0.));
#19764=DIRECTION('center_axis',(1.,0.,0.));
#19765=DIRECTION('ref_axis',(0.,1.,-2.86062230339267E-13));
#19766=DIRECTION('',(1.,0.,0.));
#19767=DIRECTION('center_axis',(1.,0.,0.));
#19768=DIRECTION('ref_axis',(0.,1.,-2.86062230339267E-13));
#19769=DIRECTION('',(1.,0.,0.));
#19770=DIRECTION('center_axis',(1.,0.,0.));
#19771=DIRECTION('ref_axis',(0.,1.,-2.86062230339267E-13));
#19772=DIRECTION('',(1.,0.,0.));
#19773=DIRECTION('center_axis',(1.,0.,0.));
#19774=DIRECTION('ref_axis',(0.,1.,-2.86062230339267E-13));
#19775=DIRECTION('',(1.,0.,0.));
#19776=DIRECTION('center_axis',(1.,0.,0.));
#19777=DIRECTION('ref_axis',(0.,1.,-2.86062230339267E-13));
#19778=DIRECTION('',(1.,0.,0.));
#19779=DIRECTION('center_axis',(1.,0.,0.));
#19780=DIRECTION('ref_axis',(0.,1.,-2.86062230339267E-13));
#19781=DIRECTION('',(1.,0.,0.));
#19782=DIRECTION('center_axis',(1.,0.,0.));
#19783=DIRECTION('ref_axis',(0.,1.,-2.86062230339267E-13));
#19784=DIRECTION('',(1.,0.,0.));
#19785=DIRECTION('center_axis',(1.,0.,0.));
#19786=DIRECTION('ref_axis',(0.,1.,-2.86062230339267E-13));
#19787=DIRECTION('',(1.,0.,0.));
#19788=DIRECTION('center_axis',(1.,0.,0.));
#19789=DIRECTION('ref_axis',(0.,1.,-2.86062230339267E-13));
#19790=DIRECTION('',(1.,0.,0.));
#19791=DIRECTION('center_axis',(1.,0.,0.));
#19792=DIRECTION('ref_axis',(0.,1.,-2.86062230339267E-13));
#19793=DIRECTION('',(1.,0.,0.));
#19794=DIRECTION('center_axis',(1.,0.,0.));
#19795=DIRECTION('ref_axis',(0.,1.,-2.86062230339267E-13));
#19796=DIRECTION('',(1.,0.,0.));
#19797=DIRECTION('center_axis',(1.,0.,0.));
#19798=DIRECTION('ref_axis',(0.,1.,-2.86062230339267E-13));
#19799=DIRECTION('',(1.,0.,0.));
#19800=DIRECTION('center_axis',(1.,0.,0.));
#19801=DIRECTION('ref_axis',(0.,1.,-2.86062230339267E-13));
#19802=DIRECTION('',(1.,0.,0.));
#19803=DIRECTION('center_axis',(1.,0.,0.));
#19804=DIRECTION('ref_axis',(0.,1.,-2.86062230339267E-13));
#19805=DIRECTION('',(1.,0.,0.));
#19806=DIRECTION('center_axis',(1.,0.,0.));
#19807=DIRECTION('ref_axis',(0.,1.,-2.86062230339267E-13));
#19808=DIRECTION('',(1.,0.,0.));
#19809=DIRECTION('center_axis',(1.,0.,0.));
#19810=DIRECTION('ref_axis',(0.,1.,-2.86062230339267E-13));
#19811=DIRECTION('',(1.,0.,0.));
#19812=DIRECTION('center_axis',(1.,0.,0.));
#19813=DIRECTION('ref_axis',(0.,1.,-2.86062230339267E-13));
#19814=DIRECTION('',(1.,0.,0.));
#19815=DIRECTION('center_axis',(1.,0.,0.));
#19816=DIRECTION('ref_axis',(0.,1.,-2.86062230339267E-13));
#19817=DIRECTION('',(1.,0.,0.));
#19818=DIRECTION('center_axis',(1.,0.,0.));
#19819=DIRECTION('ref_axis',(0.,1.,-2.86062230339267E-13));
#19820=DIRECTION('',(1.,0.,0.));
#19821=DIRECTION('center_axis',(1.,0.,0.));
#19822=DIRECTION('ref_axis',(0.,0.,-1.));
#19823=DIRECTION('center_axis',(1.,0.,0.));
#19824=DIRECTION('ref_axis',(0.,1.,0.));
#19825=DIRECTION('center_axis',(1.,0.,0.));
#19826=DIRECTION('ref_axis',(0.,1.,0.));
#19827=DIRECTION('center_axis',(-1.,0.,0.));
#19828=DIRECTION('ref_axis',(0.,1.,-2.86062230339267E-13));
#19829=DIRECTION('center_axis',(1.,0.,0.));
#19830=DIRECTION('ref_axis',(0.,0.889074354998743,0.457762811162691));
#19831=DIRECTION('center_axis',(0.,-0.45196610967378,0.892035109009925));
#19832=DIRECTION('ref_axis',(0.,-0.892035109009925,-0.45196610967378));
#19833=DIRECTION('',(-1.,0.,0.));
#19834=DIRECTION('',(0.,-0.892035109009925,-0.45196610967378));
#19835=DIRECTION('',(1.,0.,0.));
#19836=DIRECTION('',(0.,-0.892035109009925,-0.45196610967378));
#19837=DIRECTION('center_axis',(1.,0.,0.));
#19838=DIRECTION('ref_axis',(0.,-0.17364817766693,-0.984807753012208));
#19839=DIRECTION('center_axis',(-1.,0.,0.));
#19840=DIRECTION('ref_axis',(0.,1.,0.));
#19841=DIRECTION('',(0.,0.683657295809609,-0.729803193940869));
#19842=DIRECTION('center_axis',(0.,-0.729803193940869,-0.683657295809609));
#19843=DIRECTION('ref_axis',(0.,0.683657295809609,-0.729803193940869));
#19844=DIRECTION('',(1.,0.,0.));
#19845=DIRECTION('',(0.,0.683657295809609,-0.729803193940869));
#19846=DIRECTION('center_axis',(1.,0.,0.));
#19847=DIRECTION('ref_axis',(0.,-0.17364817766693,-0.984807753012208));
#19848=DIRECTION('center_axis',(1.,0.,0.));
#19849=DIRECTION('ref_axis',(0.,1.,0.));
#19850=DIRECTION('center_axis',(0.,-0.290199457811009,0.956966182624128));
#19851=DIRECTION('ref_axis',(0.,-0.956966182624128,-0.290199457811009));
#19852=DIRECTION('',(-1.,0.,0.));
#19853=DIRECTION('',(0.,-0.956966182624128,-0.290199457811009));
#19854=DIRECTION('',(1.,0.,0.));
#19855=DIRECTION('',(0.,-0.956966182624128,-0.290199457811009));
#19856=DIRECTION('center_axis',(1.,0.,0.));
#19857=DIRECTION('ref_axis',(0.,-0.342020143325669,-0.939692620785908));
#19858=DIRECTION('center_axis',(-1.,0.,0.));
#19859=DIRECTION('ref_axis',(0.,1.,0.));
#19860=DIRECTION('',(0.,0.546542010633325,-0.83743168713208));
#19861=DIRECTION('center_axis',(0.,-0.83743168713208,-0.546542010633325));
#19862=DIRECTION('ref_axis',(0.,0.546542010633325,-0.83743168713208));
#19863=DIRECTION('',(1.,0.,0.));
#19864=DIRECTION('',(0.,0.546542010633325,-0.83743168713208));
#19865=DIRECTION('center_axis',(1.,0.,0.));
#19866=DIRECTION('ref_axis',(0.,-0.342020143325669,-0.939692620785908));
#19867=DIRECTION('center_axis',(1.,0.,0.));
#19868=DIRECTION('ref_axis',(0.,1.,0.));
#19869=DIRECTION('center_axis',(0.,-0.119615242270662,0.992820323027551));
#19870=DIRECTION('ref_axis',(0.,-0.992820323027551,-0.119615242270662));
#19871=DIRECTION('',(-1.,0.,0.));
#19872=DIRECTION('',(0.,-0.992820323027551,-0.119615242270662));
#19873=DIRECTION('',(1.,0.,0.));
#19874=DIRECTION('',(0.,-0.992820323027551,-0.119615242270662));
#19875=DIRECTION('center_axis',(1.,0.,0.));
#19876=DIRECTION('ref_axis',(0.,-0.5,-0.866025403784438));
#19877=DIRECTION('center_axis',(-1.,0.,0.));
#19878=DIRECTION('ref_axis',(0.,1.,0.));
#19879=DIRECTION('',(0.,0.392820323027551,-0.919615242270663));
#19880=DIRECTION('center_axis',(0.,-0.919615242270663,-0.392820323027551));
#19881=DIRECTION('ref_axis',(0.,0.392820323027551,-0.919615242270663));
#19882=DIRECTION('',(1.,0.,0.));
#19883=DIRECTION('',(0.,0.392820323027551,-0.919615242270663));
#19884=DIRECTION('center_axis',(1.,0.,0.));
#19885=DIRECTION('ref_axis',(0.,-0.5,-0.866025403784438));
#19886=DIRECTION('center_axis',(1.,0.,0.));
#19887=DIRECTION('ref_axis',(0.,1.,0.));
#19888=DIRECTION('center_axis',(0.,0.0546034218778454,0.998508120307106));
#19889=DIRECTION('ref_axis',(0.,-0.998508120307106,0.0546034218778454));
#19890=DIRECTION('',(-1.,0.,0.));
#19891=DIRECTION('',(0.,-0.998508120307106,0.0546034218778454));
#19892=DIRECTION('',(1.,0.,0.));
#19893=DIRECTION('',(0.,-0.998508120307106,0.0546034218778454));
#19894=DIRECTION('center_axis',(1.,0.,0.));
#19895=DIRECTION('ref_axis',(0.,-0.64278760968654,-0.766044443118978));
#19896=DIRECTION('center_axis',(-1.,0.,0.));
#19897=DIRECTION('ref_axis',(0.,1.,0.));
#19898=DIRECTION('',(0.,0.227162988683259,-0.973856753620618));
#19899=DIRECTION('center_axis',(0.,-0.973856753620618,-0.227162988683259));
#19900=DIRECTION('ref_axis',(0.,0.227162988683259,-0.973856753620618));
#19901=DIRECTION('',(1.,0.,0.));
#19902=DIRECTION('',(0.,0.227162988683259,-0.973856753620618));
#19903=DIRECTION('center_axis',(1.,0.,0.));
#19904=DIRECTION('ref_axis',(0.,-0.64278760968654,-0.766044443118978));
#19905=DIRECTION('center_axis',(1.,0.,0.));
#19906=DIRECTION('ref_axis',(0.,1.,0.));
#19907=DIRECTION('center_axis',(0.,0.227162988683259,0.973856753620618));
#19908=DIRECTION('ref_axis',(0.,-0.973856753620618,0.227162988683259));
#19909=DIRECTION('',(-1.,0.,0.));
#19910=DIRECTION('',(0.,-0.973856753620618,0.227162988683259));
#19911=DIRECTION('',(1.,0.,0.));
#19912=DIRECTION('',(0.,-0.973856753620618,0.227162988683259));
#19913=DIRECTION('center_axis',(1.,0.,0.));
#19914=DIRECTION('ref_axis',(0.,-0.766044443118978,-0.642787609686539));
#19915=DIRECTION('center_axis',(-1.,0.,0.));
#19916=DIRECTION('ref_axis',(0.,1.,0.));
#19917=DIRECTION('',(0.,0.054603421877845,-0.998508120307106));
#19918=DIRECTION('center_axis',(0.,-0.998508120307106,-0.054603421877845));
#19919=DIRECTION('ref_axis',(0.,0.054603421877845,-0.998508120307106));
#19920=DIRECTION('',(1.,0.,0.));
#19921=DIRECTION('',(0.,0.054603421877845,-0.998508120307106));
#19922=DIRECTION('center_axis',(1.,0.,0.));
#19923=DIRECTION('ref_axis',(0.,-0.766044443118978,-0.642787609686539));
#19924=DIRECTION('center_axis',(1.,0.,0.));
#19925=DIRECTION('ref_axis',(0.,1.,0.));
#19926=DIRECTION('center_axis',(0.,0.392820323027551,0.919615242270663));
#19927=DIRECTION('ref_axis',(0.,-0.919615242270663,0.392820323027551));
#19928=DIRECTION('',(-1.,0.,0.));
#19929=DIRECTION('',(0.,-0.919615242270663,0.392820323027551));
#19930=DIRECTION('',(1.,0.,0.));
#19931=DIRECTION('',(0.,-0.919615242270663,0.392820323027551));
#19932=DIRECTION('center_axis',(1.,0.,0.));
#19933=DIRECTION('ref_axis',(0.,-0.866025403784439,-0.5));
#19934=DIRECTION('center_axis',(-1.,0.,0.));
#19935=DIRECTION('ref_axis',(0.,1.,0.));
#19936=DIRECTION('',(0.,-0.119615242270663,-0.992820323027551));
#19937=DIRECTION('center_axis',(0.,-0.992820323027551,0.119615242270663));
#19938=DIRECTION('ref_axis',(0.,-0.119615242270663,-0.992820323027551));
#19939=DIRECTION('',(1.,0.,0.));
#19940=DIRECTION('',(0.,-0.119615242270663,-0.992820323027551));
#19941=DIRECTION('center_axis',(1.,0.,0.));
#19942=DIRECTION('ref_axis',(0.,-0.866025403784439,-0.5));
#19943=DIRECTION('center_axis',(1.,0.,0.));
#19944=DIRECTION('ref_axis',(0.,1.,0.));
#19945=DIRECTION('center_axis',(0.,0.546542010633326,0.837431687132079));
#19946=DIRECTION('ref_axis',(0.,-0.837431687132079,0.546542010633326));
#19947=DIRECTION('',(-1.,0.,0.));
#19948=DIRECTION('',(0.,-0.837431687132079,0.546542010633326));
#19949=DIRECTION('',(1.,0.,0.));
#19950=DIRECTION('',(0.,-0.837431687132079,0.546542010633326));
#19951=DIRECTION('center_axis',(1.,0.,0.));
#19952=DIRECTION('ref_axis',(0.,-0.939692620785909,-0.342020143325668));
#19953=DIRECTION('center_axis',(-1.,0.,0.));
#19954=DIRECTION('ref_axis',(0.,1.,0.));
#19955=DIRECTION('',(0.,-0.29019945781101,-0.956966182624128));
#19956=DIRECTION('center_axis',(0.,-0.956966182624128,0.29019945781101));
#19957=DIRECTION('ref_axis',(0.,-0.29019945781101,-0.956966182624128));
#19958=DIRECTION('',(1.,0.,0.));
#19959=DIRECTION('',(0.,-0.29019945781101,-0.956966182624128));
#19960=DIRECTION('center_axis',(1.,0.,0.));
#19961=DIRECTION('ref_axis',(0.,-0.939692620785909,-0.342020143325668));
#19962=DIRECTION('center_axis',(1.,0.,0.));
#19963=DIRECTION('ref_axis',(0.,1.,0.));
#19964=DIRECTION('center_axis',(0.,0.683657295809609,0.729803193940869));
#19965=DIRECTION('ref_axis',(0.,-0.729803193940869,0.683657295809609));
#19966=DIRECTION('',(-1.,0.,0.));
#19967=DIRECTION('',(0.,-0.729803193940869,0.683657295809609));
#19968=DIRECTION('',(1.,0.,0.));
#19969=DIRECTION('',(0.,-0.729803193940869,0.683657295809609));
#19970=DIRECTION('center_axis',(1.,0.,0.));
#19971=DIRECTION('ref_axis',(0.,-0.984807753012208,-0.17364817766693));
#19972=DIRECTION('center_axis',(-1.,0.,0.));
#19973=DIRECTION('ref_axis',(0.,1.,0.));
#19974=DIRECTION('',(0.,-0.45196610967378,-0.892035109009925));
#19975=DIRECTION('center_axis',(0.,-0.892035109009925,0.451966109673781));
#19976=DIRECTION('ref_axis',(0.,-0.45196610967378,-0.892035109009925));
#19977=DIRECTION('',(1.,0.,0.));
#19978=DIRECTION('',(0.,-0.45196610967378,-0.892035109009925));
#19979=DIRECTION('center_axis',(1.,0.,0.));
#19980=DIRECTION('ref_axis',(0.,-0.984807753012208,-0.17364817766693));
#19981=DIRECTION('center_axis',(1.,0.,0.));
#19982=DIRECTION('ref_axis',(0.,1.,0.));
#19983=DIRECTION('center_axis',(0.,0.8,0.6));
#19984=DIRECTION('ref_axis',(0.,-0.6,0.8));
#19985=DIRECTION('',(-1.,0.,0.));
#19986=DIRECTION('',(0.,-0.6,0.8));
#19987=DIRECTION('',(1.,0.,0.));
#19988=DIRECTION('',(0.,-0.6,0.8));
#19989=DIRECTION('center_axis',(1.,0.,0.));
#19990=DIRECTION('ref_axis',(0.,-1.,1.83697019872103E-16));
#19991=DIRECTION('center_axis',(-1.,0.,0.));
#19992=DIRECTION('ref_axis',(0.,1.,0.));
#19993=DIRECTION('',(0.,-0.6,-0.8));
#19994=DIRECTION('center_axis',(0.,-0.8,0.6));
#19995=DIRECTION('ref_axis',(0.,-0.6,-0.8));
#19996=DIRECTION('',(1.,0.,0.));
#19997=DIRECTION('',(0.,-0.6,-0.8));
#19998=DIRECTION('center_axis',(1.,0.,0.));
#19999=DIRECTION('ref_axis',(0.,-1.,1.83697019872103E-16));
#20000=DIRECTION('center_axis',(1.,0.,0.));
#20001=DIRECTION('ref_axis',(0.,1.,0.));
#20002=DIRECTION('center_axis',(0.,0.892035109009925,0.45196610967378));
#20003=DIRECTION('ref_axis',(0.,-0.45196610967378,0.892035109009925));
#20004=DIRECTION('',(-1.,0.,0.));
#20005=DIRECTION('',(0.,-0.45196610967378,0.892035109009925));
#20006=DIRECTION('',(1.,0.,0.));
#20007=DIRECTION('',(0.,-0.45196610967378,0.892035109009925));
#20008=DIRECTION('center_axis',(1.,0.,0.));
#20009=DIRECTION('ref_axis',(0.,-0.984807753012208,0.17364817766693));
#20010=DIRECTION('center_axis',(-1.,0.,0.));
#20011=DIRECTION('ref_axis',(0.,1.,0.));
#20012=DIRECTION('',(0.,-0.729803193940869,-0.683657295809609));
#20013=DIRECTION('center_axis',(0.,-0.683657295809609,0.729803193940869));
#20014=DIRECTION('ref_axis',(0.,-0.729803193940869,-0.683657295809609));
#20015=DIRECTION('',(1.,0.,0.));
#20016=DIRECTION('',(0.,-0.729803193940869,-0.683657295809609));
#20017=DIRECTION('center_axis',(1.,0.,0.));
#20018=DIRECTION('ref_axis',(0.,-0.984807753012208,0.17364817766693));
#20019=DIRECTION('center_axis',(1.,0.,0.));
#20020=DIRECTION('ref_axis',(0.,1.,0.));
#20021=DIRECTION('center_axis',(0.,0.956966182624128,0.290199457811009));
#20022=DIRECTION('ref_axis',(0.,-0.290199457811009,0.956966182624128));
#20023=DIRECTION('',(-1.,0.,0.));
#20024=DIRECTION('',(0.,-0.290199457811009,0.956966182624128));
#20025=DIRECTION('',(1.,0.,0.));
#20026=DIRECTION('',(0.,-0.290199457811009,0.956966182624128));
#20027=DIRECTION('center_axis',(1.,0.,0.));
#20028=DIRECTION('ref_axis',(0.,-0.939692620785908,0.342020143325669));
#20029=DIRECTION('center_axis',(-1.,0.,0.));
#20030=DIRECTION('ref_axis',(0.,1.,0.));
#20031=DIRECTION('',(0.,-0.83743168713208,-0.546542010633325));
#20032=DIRECTION('center_axis',(0.,-0.546542010633325,0.83743168713208));
#20033=DIRECTION('ref_axis',(0.,-0.83743168713208,-0.546542010633325));
#20034=DIRECTION('',(1.,0.,0.));
#20035=DIRECTION('',(0.,-0.83743168713208,-0.546542010633325));
#20036=DIRECTION('center_axis',(1.,0.,0.));
#20037=DIRECTION('ref_axis',(0.,-0.939692620785908,0.342020143325669));
#20038=DIRECTION('center_axis',(1.,0.,0.));
#20039=DIRECTION('ref_axis',(0.,1.,0.));
#20040=DIRECTION('center_axis',(0.,0.992820323027551,0.119615242270662));
#20041=DIRECTION('ref_axis',(0.,-0.119615242270662,0.992820323027551));
#20042=DIRECTION('',(-1.,0.,0.));
#20043=DIRECTION('',(0.,-0.119615242270662,0.992820323027551));
#20044=DIRECTION('',(1.,0.,0.));
#20045=DIRECTION('',(0.,-0.119615242270662,0.992820323027551));
#20046=DIRECTION('center_axis',(1.,0.,0.));
#20047=DIRECTION('ref_axis',(0.,-0.866025403784438,0.5));
#20048=DIRECTION('center_axis',(-1.,0.,0.));
#20049=DIRECTION('ref_axis',(0.,1.,0.));
#20050=DIRECTION('',(0.,-0.919615242270663,-0.392820323027551));
#20051=DIRECTION('center_axis',(0.,-0.392820323027551,0.919615242270663));
#20052=DIRECTION('ref_axis',(0.,-0.919615242270663,-0.392820323027551));
#20053=DIRECTION('',(1.,0.,0.));
#20054=DIRECTION('',(0.,-0.919615242270663,-0.392820323027551));
#20055=DIRECTION('center_axis',(1.,0.,0.));
#20056=DIRECTION('ref_axis',(0.,-0.866025403784438,0.5));
#20057=DIRECTION('center_axis',(1.,0.,0.));
#20058=DIRECTION('ref_axis',(0.,1.,0.));
#20059=DIRECTION('center_axis',(0.,0.998508120307106,-0.0546034218778453));
#20060=DIRECTION('ref_axis',(0.,0.0546034218778453,0.998508120307106));
#20061=DIRECTION('',(-1.,0.,0.));
#20062=DIRECTION('',(0.,0.0546034218778453,0.998508120307106));
#20063=DIRECTION('',(1.,0.,0.));
#20064=DIRECTION('',(0.,0.0546034218778453,0.998508120307106));
#20065=DIRECTION('center_axis',(1.,0.,0.));
#20066=DIRECTION('ref_axis',(0.,-0.766044443118978,0.642787609686539));
#20067=DIRECTION('center_axis',(-1.,0.,0.));
#20068=DIRECTION('ref_axis',(0.,1.,0.));
#20069=DIRECTION('',(0.,-0.973856753620618,-0.227162988683259));
#20070=DIRECTION('center_axis',(0.,-0.227162988683259,0.973856753620618));
#20071=DIRECTION('ref_axis',(0.,-0.973856753620618,-0.227162988683259));
#20072=DIRECTION('',(1.,0.,0.));
#20073=DIRECTION('',(0.,-0.973856753620618,-0.227162988683259));
#20074=DIRECTION('center_axis',(1.,0.,0.));
#20075=DIRECTION('ref_axis',(0.,-0.766044443118978,0.642787609686539));
#20076=DIRECTION('center_axis',(1.,0.,0.));
#20077=DIRECTION('ref_axis',(0.,1.,0.));
#20078=DIRECTION('center_axis',(0.,0.973856753620618,-0.227162988683259));
#20079=DIRECTION('ref_axis',(0.,0.227162988683259,0.973856753620618));
#20080=DIRECTION('',(-1.,0.,0.));
#20081=DIRECTION('',(0.,0.227162988683259,0.973856753620618));
#20082=DIRECTION('',(1.,0.,0.));
#20083=DIRECTION('',(0.,0.227162988683259,0.973856753620618));
#20084=DIRECTION('center_axis',(1.,0.,0.));
#20085=DIRECTION('ref_axis',(0.,-0.642787609686539,0.766044443118978));
#20086=DIRECTION('center_axis',(-1.,0.,0.));
#20087=DIRECTION('ref_axis',(0.,1.,0.));
#20088=DIRECTION('',(0.,-0.998508120307106,-0.054603421877845));
#20089=DIRECTION('center_axis',(0.,-0.054603421877845,0.998508120307106));
#20090=DIRECTION('ref_axis',(0.,-0.998508120307106,-0.054603421877845));
#20091=DIRECTION('',(1.,0.,0.));
#20092=DIRECTION('',(0.,-0.998508120307106,-0.054603421877845));
#20093=DIRECTION('center_axis',(1.,0.,0.));
#20094=DIRECTION('ref_axis',(0.,-0.642787609686539,0.766044443118978));
#20095=DIRECTION('center_axis',(1.,0.,0.));
#20096=DIRECTION('ref_axis',(0.,1.,0.));
#20097=DIRECTION('center_axis',(0.,0.919615242270663,-0.392820323027552));
#20098=DIRECTION('ref_axis',(0.,0.392820323027552,0.919615242270663));
#20099=DIRECTION('',(-1.,0.,0.));
#20100=DIRECTION('',(0.,0.392820323027552,0.919615242270663));
#20101=DIRECTION('',(1.,0.,0.));
#20102=DIRECTION('',(0.,0.392820323027552,0.919615242270663));
#20103=DIRECTION('center_axis',(1.,0.,0.));
#20104=DIRECTION('ref_axis',(0.,-0.5,0.866025403784439));
#20105=DIRECTION('center_axis',(-1.,0.,0.));
#20106=DIRECTION('ref_axis',(0.,1.,0.));
#20107=DIRECTION('',(0.,-0.992820323027551,0.119615242270663));
#20108=DIRECTION('center_axis',(0.,0.119615242270663,0.992820323027551));
#20109=DIRECTION('ref_axis',(0.,-0.992820323027551,0.119615242270663));
#20110=DIRECTION('',(1.,0.,0.));
#20111=DIRECTION('',(0.,-0.992820323027551,0.119615242270663));
#20112=DIRECTION('center_axis',(1.,0.,0.));
#20113=DIRECTION('ref_axis',(0.,-0.5,0.866025403784439));
#20114=DIRECTION('center_axis',(1.,0.,0.));
#20115=DIRECTION('ref_axis',(0.,1.,0.));
#20116=DIRECTION('center_axis',(0.,0.83743168713208,-0.546542010633326));
#20117=DIRECTION('ref_axis',(0.,0.546542010633326,0.83743168713208));
#20118=DIRECTION('',(-1.,0.,0.));
#20119=DIRECTION('',(0.,0.546542010633326,0.83743168713208));
#20120=DIRECTION('',(1.,0.,0.));
#20121=DIRECTION('',(0.,0.546542010633326,0.83743168713208));
#20122=DIRECTION('center_axis',(1.,0.,0.));
#20123=DIRECTION('ref_axis',(0.,-0.342020143325669,0.939692620785909));
#20124=DIRECTION('center_axis',(-1.,0.,0.));
#20125=DIRECTION('ref_axis',(0.,1.,0.));
#20126=DIRECTION('',(0.,-0.956966182624128,0.29019945781101));
#20127=DIRECTION('center_axis',(0.,0.29019945781101,0.956966182624128));
#20128=DIRECTION('ref_axis',(0.,-0.956966182624128,0.29019945781101));
#20129=DIRECTION('',(1.,0.,0.));
#20130=DIRECTION('',(0.,-0.956966182624128,0.29019945781101));
#20131=DIRECTION('center_axis',(1.,0.,0.));
#20132=DIRECTION('ref_axis',(0.,-0.342020143325669,0.939692620785909));
#20133=DIRECTION('center_axis',(1.,0.,0.));
#20134=DIRECTION('ref_axis',(0.,1.,0.));
#20135=DIRECTION('center_axis',(0.,0.729803193940869,-0.683657295809609));
#20136=DIRECTION('ref_axis',(0.,0.683657295809609,0.729803193940869));
#20137=DIRECTION('',(-1.,0.,0.));
#20138=DIRECTION('',(0.,0.683657295809609,0.729803193940869));
#20139=DIRECTION('',(1.,0.,0.));
#20140=DIRECTION('',(0.,0.683657295809609,0.729803193940869));
#20141=DIRECTION('center_axis',(1.,0.,0.));
#20142=DIRECTION('ref_axis',(0.,-0.17364817766693,0.984807753012208));
#20143=DIRECTION('center_axis',(-1.,0.,0.));
#20144=DIRECTION('ref_axis',(0.,1.,0.));
#20145=DIRECTION('',(0.,-0.892035109009925,0.45196610967378));
#20146=DIRECTION('center_axis',(0.,0.45196610967378,0.892035109009925));
#20147=DIRECTION('ref_axis',(0.,-0.892035109009925,0.45196610967378));
#20148=DIRECTION('',(1.,0.,0.));
#20149=DIRECTION('',(0.,-0.892035109009925,0.45196610967378));
#20150=DIRECTION('center_axis',(1.,0.,0.));
#20151=DIRECTION('ref_axis',(0.,-0.17364817766693,0.984807753012208));
#20152=DIRECTION('center_axis',(1.,0.,0.));
#20153=DIRECTION('ref_axis',(0.,1.,0.));
#20154=DIRECTION('center_axis',(0.,0.6,-0.8));
#20155=DIRECTION('ref_axis',(0.,0.8,0.6));
#20156=DIRECTION('',(-1.,0.,0.));
#20157=DIRECTION('',(0.,0.8,0.6));
#20158=DIRECTION('',(1.,0.,0.));
#20159=DIRECTION('',(0.,0.8,0.6));
#20160=DIRECTION('center_axis',(1.,0.,0.));
#20161=DIRECTION('ref_axis',(0.,1.22464679914735E-16,1.));
#20162=DIRECTION('center_axis',(-1.,0.,0.));
#20163=DIRECTION('ref_axis',(0.,1.,0.));
#20164=DIRECTION('',(0.,-0.8,0.6));
#20165=DIRECTION('center_axis',(-1.,0.,0.));
#20166=DIRECTION('ref_axis',(0.,1.,0.));
#20167=DIRECTION('center_axis',(0.,0.6,0.8));
#20168=DIRECTION('ref_axis',(0.,-0.8,0.6));
#20169=DIRECTION('',(1.,0.,0.));
#20170=DIRECTION('',(0.,-0.8,0.6));
#20171=DIRECTION('center_axis',(1.,0.,0.));
#20172=DIRECTION('ref_axis',(0.,1.22464679914735E-16,1.));
#20173=DIRECTION('center_axis',(1.,0.,0.));
#20174=DIRECTION('ref_axis',(0.,1.,0.));
#20175=DIRECTION('center_axis',(1.,0.,0.));
#20176=DIRECTION('ref_axis',(0.,1.,0.));
#20177=DIRECTION('center_axis',(0.,0.45196610967378,-0.892035109009925));
#20178=DIRECTION('ref_axis',(0.,0.892035109009925,0.45196610967378));
#20179=DIRECTION('',(-1.,0.,0.));
#20180=DIRECTION('',(0.,0.892035109009925,0.45196610967378));
#20181=DIRECTION('',(1.,0.,0.));
#20182=DIRECTION('',(0.,0.892035109009925,0.45196610967378));
#20183=DIRECTION('center_axis',(1.,0.,0.));
#20184=DIRECTION('ref_axis',(0.,0.173648177666931,0.984807753012208));
#20185=DIRECTION('center_axis',(-1.,0.,0.));
#20186=DIRECTION('ref_axis',(0.,1.,0.));
#20187=DIRECTION('',(0.,-0.683657295809608,0.729803193940869));
#20188=DIRECTION('center_axis',(0.,0.729803193940869,0.683657295809608));
#20189=DIRECTION('ref_axis',(0.,-0.683657295809608,0.729803193940869));
#20190=DIRECTION('',(1.,0.,0.));
#20191=DIRECTION('',(0.,-0.683657295809608,0.729803193940869));
#20192=DIRECTION('center_axis',(1.,0.,0.));
#20193=DIRECTION('ref_axis',(0.,0.173648177666931,0.984807753012208));
#20194=DIRECTION('center_axis',(1.,0.,0.));
#20195=DIRECTION('ref_axis',(0.,1.,0.));
#20196=DIRECTION('center_axis',(0.,0.290199457811009,-0.956966182624128));
#20197=DIRECTION('ref_axis',(0.,0.956966182624128,0.290199457811009));
#20198=DIRECTION('',(-1.,0.,0.));
#20199=DIRECTION('',(0.,0.956966182624128,0.290199457811009));
#20200=DIRECTION('',(1.,0.,0.));
#20201=DIRECTION('',(0.,0.956966182624128,0.290199457811009));
#20202=DIRECTION('center_axis',(1.,0.,0.));
#20203=DIRECTION('ref_axis',(0.,0.342020143325669,0.939692620785908));
#20204=DIRECTION('center_axis',(-1.,0.,0.));
#20205=DIRECTION('ref_axis',(0.,1.,0.));
#20206=DIRECTION('',(0.,-0.546542010633326,0.83743168713208));
#20207=DIRECTION('center_axis',(0.,0.83743168713208,0.546542010633326));
#20208=DIRECTION('ref_axis',(0.,-0.546542010633326,0.83743168713208));
#20209=DIRECTION('',(1.,0.,0.));
#20210=DIRECTION('',(0.,-0.546542010633326,0.83743168713208));
#20211=DIRECTION('center_axis',(1.,0.,0.));
#20212=DIRECTION('ref_axis',(0.,0.342020143325669,0.939692620785908));
#20213=DIRECTION('center_axis',(1.,0.,0.));
#20214=DIRECTION('ref_axis',(0.,1.,0.));
#20215=DIRECTION('center_axis',(0.,0.119615242270663,-0.992820323027551));
#20216=DIRECTION('ref_axis',(0.,0.992820323027551,0.119615242270663));
#20217=DIRECTION('',(-1.,0.,0.));
#20218=DIRECTION('',(0.,0.992820323027551,0.119615242270663));
#20219=DIRECTION('',(1.,0.,0.));
#20220=DIRECTION('',(0.,0.992820323027551,0.119615242270663));
#20221=DIRECTION('center_axis',(1.,0.,0.));
#20222=DIRECTION('ref_axis',(0.,0.5,0.866025403784439));
#20223=DIRECTION('center_axis',(-1.,0.,0.));
#20224=DIRECTION('ref_axis',(0.,1.,0.));
#20225=DIRECTION('',(0.,-0.392820323027551,0.919615242270663));
#20226=DIRECTION('center_axis',(0.,0.919615242270663,0.392820323027551));
#20227=DIRECTION('ref_axis',(0.,-0.392820323027551,0.919615242270663));
#20228=DIRECTION('',(1.,0.,0.));
#20229=DIRECTION('',(0.,-0.392820323027551,0.919615242270663));
#20230=DIRECTION('center_axis',(1.,0.,0.));
#20231=DIRECTION('ref_axis',(0.,0.5,0.866025403784439));
#20232=DIRECTION('center_axis',(1.,0.,0.));
#20233=DIRECTION('ref_axis',(0.,1.,0.));
#20234=DIRECTION('center_axis',(0.,-0.0546034218778453,-0.998508120307106));
#20235=DIRECTION('ref_axis',(0.,0.998508120307106,-0.0546034218778453));
#20236=DIRECTION('',(-1.,0.,0.));
#20237=DIRECTION('',(0.,0.998508120307106,-0.0546034218778453));
#20238=DIRECTION('',(1.,0.,0.));
#20239=DIRECTION('',(0.,0.998508120307106,-0.0546034218778453));
#20240=DIRECTION('center_axis',(1.,0.,0.));
#20241=DIRECTION('ref_axis',(0.,0.642787609686539,0.766044443118978));
#20242=DIRECTION('center_axis',(-1.,0.,0.));
#20243=DIRECTION('ref_axis',(0.,1.,0.));
#20244=DIRECTION('',(0.,-0.227162988683259,0.973856753620618));
#20245=DIRECTION('center_axis',(0.,0.973856753620618,0.227162988683259));
#20246=DIRECTION('ref_axis',(0.,-0.227162988683259,0.973856753620618));
#20247=DIRECTION('',(1.,0.,0.));
#20248=DIRECTION('',(0.,-0.227162988683259,0.973856753620618));
#20249=DIRECTION('center_axis',(1.,0.,0.));
#20250=DIRECTION('ref_axis',(0.,0.642787609686539,0.766044443118978));
#20251=DIRECTION('center_axis',(1.,0.,0.));
#20252=DIRECTION('ref_axis',(0.,1.,0.));
#20253=DIRECTION('center_axis',(0.,-0.227162988683259,-0.973856753620618));
#20254=DIRECTION('ref_axis',(0.,0.973856753620618,-0.227162988683259));
#20255=DIRECTION('',(-1.,0.,0.));
#20256=DIRECTION('',(0.,0.973856753620618,-0.227162988683259));
#20257=DIRECTION('',(1.,0.,0.));
#20258=DIRECTION('',(0.,0.973856753620618,-0.227162988683259));
#20259=DIRECTION('center_axis',(1.,0.,0.));
#20260=DIRECTION('ref_axis',(0.,0.766044443118978,0.642787609686539));
#20261=DIRECTION('center_axis',(-1.,0.,0.));
#20262=DIRECTION('ref_axis',(0.,1.,0.));
#20263=DIRECTION('',(0.,-0.0546034218778451,0.998508120307106));
#20264=DIRECTION('center_axis',(0.,0.998508120307106,0.0546034218778451));
#20265=DIRECTION('ref_axis',(0.,-0.0546034218778451,0.998508120307106));
#20266=DIRECTION('',(1.,0.,0.));
#20267=DIRECTION('',(0.,-0.0546034218778451,0.998508120307106));
#20268=DIRECTION('center_axis',(1.,0.,0.));
#20269=DIRECTION('ref_axis',(0.,0.766044443118978,0.642787609686539));
#20270=DIRECTION('center_axis',(1.,0.,0.));
#20271=DIRECTION('ref_axis',(0.,1.,0.));
#20272=DIRECTION('center_axis',(0.,-0.392820323027552,-0.919615242270663));
#20273=DIRECTION('ref_axis',(0.,0.919615242270663,-0.392820323027551));
#20274=DIRECTION('',(-1.,0.,0.));
#20275=DIRECTION('',(0.,0.919615242270663,-0.392820323027551));
#20276=DIRECTION('',(1.,0.,0.));
#20277=DIRECTION('',(0.,0.919615242270663,-0.392820323027551));
#20278=DIRECTION('center_axis',(1.,0.,0.));
#20279=DIRECTION('ref_axis',(0.,0.866025403784439,0.5));
#20280=DIRECTION('center_axis',(-1.,0.,0.));
#20281=DIRECTION('ref_axis',(0.,1.,0.));
#20282=DIRECTION('',(0.,0.119615242270663,0.992820323027551));
#20283=DIRECTION('center_axis',(0.,0.992820323027551,-0.119615242270663));
#20284=DIRECTION('ref_axis',(0.,0.119615242270663,0.992820323027551));
#20285=DIRECTION('',(1.,0.,0.));
#20286=DIRECTION('',(0.,0.119615242270663,0.992820323027551));
#20287=DIRECTION('center_axis',(1.,0.,0.));
#20288=DIRECTION('ref_axis',(0.,0.866025403784439,0.5));
#20289=DIRECTION('center_axis',(1.,0.,0.));
#20290=DIRECTION('ref_axis',(0.,1.,0.));
#20291=DIRECTION('center_axis',(0.,-0.546542010633326,-0.83743168713208));
#20292=DIRECTION('ref_axis',(0.,0.83743168713208,-0.546542010633326));
#20293=DIRECTION('',(-1.,0.,0.));
#20294=DIRECTION('',(0.,0.83743168713208,-0.546542010633326));
#20295=DIRECTION('',(1.,0.,0.));
#20296=DIRECTION('',(0.,0.83743168713208,-0.546542010633326));
#20297=DIRECTION('center_axis',(1.,0.,0.));
#20298=DIRECTION('ref_axis',(0.,0.939692620785908,0.342020143325669));
#20299=DIRECTION('center_axis',(-1.,0.,0.));
#20300=DIRECTION('ref_axis',(0.,1.,0.));
#20301=DIRECTION('',(0.,0.29019945781101,0.956966182624128));
#20302=DIRECTION('center_axis',(0.,0.956966182624128,-0.29019945781101));
#20303=DIRECTION('ref_axis',(0.,0.29019945781101,0.956966182624128));
#20304=DIRECTION('',(1.,0.,0.));
#20305=DIRECTION('',(0.,0.29019945781101,0.956966182624128));
#20306=DIRECTION('center_axis',(1.,0.,0.));
#20307=DIRECTION('ref_axis',(0.,0.939692620785908,0.342020143325669));
#20308=DIRECTION('center_axis',(1.,0.,0.));
#20309=DIRECTION('ref_axis',(0.,1.,0.));
#20310=DIRECTION('center_axis',(0.,-0.683657295809609,-0.729803193940869));
#20311=DIRECTION('ref_axis',(0.,0.729803193940869,-0.683657295809609));
#20312=DIRECTION('',(-1.,0.,0.));
#20313=DIRECTION('',(0.,0.729803193940869,-0.683657295809609));
#20314=DIRECTION('',(1.,0.,0.));
#20315=DIRECTION('',(0.,0.729803193940869,-0.683657295809609));
#20316=DIRECTION('center_axis',(1.,0.,0.));
#20317=DIRECTION('ref_axis',(0.,0.984807753012208,0.17364817766693));
#20318=DIRECTION('center_axis',(-1.,0.,0.));
#20319=DIRECTION('ref_axis',(0.,1.,0.));
#20320=DIRECTION('',(0.,0.45196610967378,0.892035109009925));
#20321=DIRECTION('center_axis',(0.,0.892035109009925,-0.45196610967378));
#20322=DIRECTION('ref_axis',(0.,0.45196610967378,0.892035109009925));
#20323=DIRECTION('',(1.,0.,0.));
#20324=DIRECTION('',(0.,0.45196610967378,0.892035109009925));
#20325=DIRECTION('center_axis',(1.,0.,0.));
#20326=DIRECTION('ref_axis',(0.,0.984807753012208,0.17364817766693));
#20327=DIRECTION('center_axis',(1.,0.,0.));
#20328=DIRECTION('ref_axis',(0.,1.,0.));
#20329=DIRECTION('center_axis',(0.,-0.8,-0.6));
#20330=DIRECTION('ref_axis',(0.,0.6,-0.8));
#20331=DIRECTION('',(-1.,0.,0.));
#20332=DIRECTION('',(0.,0.6,-0.8));
#20333=DIRECTION('',(1.,0.,0.));
#20334=DIRECTION('',(0.,0.6,-0.8));
#20335=DIRECTION('center_axis',(1.,0.,0.));
#20336=DIRECTION('ref_axis',(0.,1.,-6.12323399573677E-17));
#20337=DIRECTION('center_axis',(-1.,0.,0.));
#20338=DIRECTION('ref_axis',(0.,1.,0.));
#20339=DIRECTION('',(0.,0.6,0.8));
#20340=DIRECTION('center_axis',(0.,0.8,-0.6));
#20341=DIRECTION('ref_axis',(0.,0.6,0.8));
#20342=DIRECTION('',(1.,0.,0.));
#20343=DIRECTION('',(0.,0.6,0.8));
#20344=DIRECTION('center_axis',(1.,0.,0.));
#20345=DIRECTION('ref_axis',(0.,1.,-6.12323399573677E-17));
#20346=DIRECTION('center_axis',(1.,0.,0.));
#20347=DIRECTION('ref_axis',(0.,1.,0.));
#20348=DIRECTION('center_axis',(0.,-0.892035109009925,-0.45196610967378));
#20349=DIRECTION('ref_axis',(0.,0.45196610967378,-0.892035109009925));
#20350=DIRECTION('',(-1.,0.,0.));
#20351=DIRECTION('',(0.,0.45196610967378,-0.892035109009925));
#20352=DIRECTION('',(1.,0.,0.));
#20353=DIRECTION('',(0.,0.45196610967378,-0.892035109009925));
#20354=DIRECTION('center_axis',(1.,0.,0.));
#20355=DIRECTION('ref_axis',(0.,0.984807753012208,-0.17364817766693));
#20356=DIRECTION('center_axis',(-1.,0.,0.));
#20357=DIRECTION('ref_axis',(0.,1.,0.));
#20358=DIRECTION('',(0.,0.729803193940869,0.683657295809609));
#20359=DIRECTION('center_axis',(0.,0.683657295809609,-0.729803193940869));
#20360=DIRECTION('ref_axis',(0.,0.729803193940869,0.683657295809609));
#20361=DIRECTION('',(1.,0.,0.));
#20362=DIRECTION('',(0.,0.729803193940869,0.683657295809609));
#20363=DIRECTION('center_axis',(1.,0.,0.));
#20364=DIRECTION('ref_axis',(0.,0.984807753012208,-0.17364817766693));
#20365=DIRECTION('center_axis',(1.,0.,0.));
#20366=DIRECTION('ref_axis',(0.,1.,0.));
#20367=DIRECTION('center_axis',(0.,-0.956966182624128,-0.290199457811009));
#20368=DIRECTION('ref_axis',(0.,0.290199457811009,-0.956966182624128));
#20369=DIRECTION('',(-1.,0.,0.));
#20370=DIRECTION('',(0.,0.290199457811009,-0.956966182624128));
#20371=DIRECTION('',(1.,0.,0.));
#20372=DIRECTION('',(0.,0.290199457811009,-0.956966182624128));
#20373=DIRECTION('center_axis',(1.,0.,0.));
#20374=DIRECTION('ref_axis',(0.,0.939692620785908,-0.342020143325669));
#20375=DIRECTION('center_axis',(-1.,0.,0.));
#20376=DIRECTION('ref_axis',(0.,1.,0.));
#20377=DIRECTION('',(0.,0.83743168713208,0.546542010633326));
#20378=DIRECTION('center_axis',(0.,0.546542010633326,-0.83743168713208));
#20379=DIRECTION('ref_axis',(0.,0.83743168713208,0.546542010633326));
#20380=DIRECTION('',(1.,0.,0.));
#20381=DIRECTION('',(0.,0.83743168713208,0.546542010633326));
#20382=DIRECTION('center_axis',(1.,0.,0.));
#20383=DIRECTION('ref_axis',(0.,0.939692620785908,-0.342020143325669));
#20384=DIRECTION('center_axis',(1.,0.,0.));
#20385=DIRECTION('ref_axis',(0.,1.,0.));
#20386=DIRECTION('center_axis',(0.,-0.992820323027551,-0.119615242270663));
#20387=DIRECTION('ref_axis',(0.,0.119615242270663,-0.992820323027551));
#20388=DIRECTION('',(-1.,0.,0.));
#20389=DIRECTION('',(0.,0.119615242270663,-0.992820323027551));
#20390=DIRECTION('',(1.,0.,0.));
#20391=DIRECTION('',(0.,0.119615242270663,-0.992820323027551));
#20392=DIRECTION('center_axis',(1.,0.,0.));
#20393=DIRECTION('ref_axis',(0.,0.866025403784439,-0.5));
#20394=DIRECTION('center_axis',(-1.,0.,0.));
#20395=DIRECTION('ref_axis',(0.,1.,0.));
#20396=DIRECTION('',(0.,0.919615242270663,0.392820323027551));
#20397=DIRECTION('center_axis',(0.,0.392820323027551,-0.919615242270663));
#20398=DIRECTION('ref_axis',(0.,0.919615242270663,0.392820323027551));
#20399=DIRECTION('',(1.,0.,0.));
#20400=DIRECTION('',(0.,0.919615242270663,0.392820323027551));
#20401=DIRECTION('center_axis',(1.,0.,0.));
#20402=DIRECTION('ref_axis',(0.,0.866025403784439,-0.5));
#20403=DIRECTION('center_axis',(1.,0.,0.));
#20404=DIRECTION('ref_axis',(0.,1.,0.));
#20405=DIRECTION('center_axis',(0.,-0.998508120307106,0.0546034218778451));
#20406=DIRECTION('ref_axis',(0.,-0.0546034218778451,-0.998508120307106));
#20407=DIRECTION('',(-1.,0.,0.));
#20408=DIRECTION('',(0.,-0.0546034218778451,-0.998508120307106));
#20409=DIRECTION('',(1.,0.,0.));
#20410=DIRECTION('',(0.,-0.0546034218778451,-0.998508120307106));
#20411=DIRECTION('center_axis',(1.,0.,0.));
#20412=DIRECTION('ref_axis',(0.,0.766044443118978,-0.642787609686539));
#20413=DIRECTION('center_axis',(-1.,0.,0.));
#20414=DIRECTION('ref_axis',(0.,1.,0.));
#20415=DIRECTION('',(0.,0.973856753620618,0.227162988683259));
#20416=DIRECTION('center_axis',(0.,0.227162988683259,-0.973856753620618));
#20417=DIRECTION('ref_axis',(0.,0.973856753620618,0.227162988683259));
#20418=DIRECTION('',(1.,0.,0.));
#20419=DIRECTION('',(0.,0.973856753620618,0.227162988683259));
#20420=DIRECTION('center_axis',(1.,0.,0.));
#20421=DIRECTION('ref_axis',(0.,0.766044443118978,-0.642787609686539));
#20422=DIRECTION('center_axis',(1.,0.,0.));
#20423=DIRECTION('ref_axis',(0.,1.,0.));
#20424=DIRECTION('center_axis',(0.,-0.973856753620618,0.227162988683259));
#20425=DIRECTION('ref_axis',(0.,-0.227162988683259,-0.973856753620618));
#20426=DIRECTION('',(-1.,0.,0.));
#20427=DIRECTION('',(0.,-0.227162988683259,-0.973856753620618));
#20428=DIRECTION('',(1.,0.,0.));
#20429=DIRECTION('',(0.,-0.227162988683259,-0.973856753620618));
#20430=DIRECTION('center_axis',(1.,0.,0.));
#20431=DIRECTION('ref_axis',(0.,0.642787609686539,-0.766044443118978));
#20432=DIRECTION('center_axis',(-1.,0.,0.));
#20433=DIRECTION('ref_axis',(0.,1.,0.));
#20434=DIRECTION('',(0.,0.998508120307106,0.054603421877845));
#20435=DIRECTION('center_axis',(0.,0.054603421877845,-0.998508120307106));
#20436=DIRECTION('ref_axis',(0.,0.998508120307106,0.054603421877845));
#20437=DIRECTION('',(1.,0.,0.));
#20438=DIRECTION('',(0.,0.998508120307106,0.054603421877845));
#20439=DIRECTION('center_axis',(1.,0.,0.));
#20440=DIRECTION('ref_axis',(0.,0.642787609686539,-0.766044443118978));
#20441=DIRECTION('center_axis',(1.,0.,0.));
#20442=DIRECTION('ref_axis',(0.,1.,0.));
#20443=DIRECTION('center_axis',(0.,-0.919615242270663,0.392820323027551));
#20444=DIRECTION('ref_axis',(0.,-0.392820323027551,-0.919615242270663));
#20445=DIRECTION('',(-1.,0.,0.));
#20446=DIRECTION('',(0.,-0.392820323027551,-0.919615242270663));
#20447=DIRECTION('',(1.,0.,0.));
#20448=DIRECTION('',(0.,-0.392820323027551,-0.919615242270663));
#20449=DIRECTION('center_axis',(1.,0.,0.));
#20450=DIRECTION('ref_axis',(0.,0.5,-0.866025403784439));
#20451=DIRECTION('center_axis',(-1.,0.,0.));
#20452=DIRECTION('ref_axis',(0.,1.,0.));
#20453=DIRECTION('',(0.,0.992820323027551,-0.119615242270663));
#20454=DIRECTION('center_axis',(0.,-0.119615242270663,-0.992820323027551));
#20455=DIRECTION('ref_axis',(0.,0.992820323027551,-0.119615242270663));
#20456=DIRECTION('',(1.,0.,0.));
#20457=DIRECTION('',(0.,0.992820323027551,-0.119615242270663));
#20458=DIRECTION('center_axis',(1.,0.,0.));
#20459=DIRECTION('ref_axis',(0.,0.5,-0.866025403784439));
#20460=DIRECTION('center_axis',(1.,0.,0.));
#20461=DIRECTION('ref_axis',(0.,1.,0.));
#20462=DIRECTION('center_axis',(0.,-0.83743168713208,0.546542010633326));
#20463=DIRECTION('ref_axis',(0.,-0.546542010633326,-0.83743168713208));
#20464=DIRECTION('',(-1.,0.,0.));
#20465=DIRECTION('',(0.,-0.546542010633326,-0.83743168713208));
#20466=DIRECTION('',(1.,0.,0.));
#20467=DIRECTION('',(0.,-0.546542010633326,-0.83743168713208));
#20468=DIRECTION('center_axis',(1.,0.,0.));
#20469=DIRECTION('ref_axis',(0.,0.342020143325669,-0.939692620785908));
#20470=DIRECTION('center_axis',(-1.,0.,0.));
#20471=DIRECTION('ref_axis',(0.,1.,0.));
#20472=DIRECTION('',(0.,0.956966182624128,-0.29019945781101));
#20473=DIRECTION('center_axis',(0.,-0.29019945781101,-0.956966182624128));
#20474=DIRECTION('ref_axis',(0.,0.956966182624128,-0.29019945781101));
#20475=DIRECTION('',(1.,0.,0.));
#20476=DIRECTION('',(0.,0.956966182624128,-0.29019945781101));
#20477=DIRECTION('center_axis',(1.,0.,0.));
#20478=DIRECTION('ref_axis',(0.,0.342020143325669,-0.939692620785908));
#20479=DIRECTION('center_axis',(1.,0.,0.));
#20480=DIRECTION('ref_axis',(0.,1.,0.));
#20481=DIRECTION('center_axis',(0.,-0.729803193940869,0.683657295809609));
#20482=DIRECTION('ref_axis',(0.,-0.683657295809609,-0.729803193940869));
#20483=DIRECTION('',(-1.,0.,0.));
#20484=DIRECTION('',(0.,-0.683657295809609,-0.729803193940869));
#20485=DIRECTION('',(1.,0.,0.));
#20486=DIRECTION('',(0.,-0.683657295809609,-0.729803193940869));
#20487=DIRECTION('center_axis',(1.,0.,0.));
#20488=DIRECTION('ref_axis',(0.,0.17364817766693,-0.984807753012208));
#20489=DIRECTION('center_axis',(-1.,0.,0.));
#20490=DIRECTION('ref_axis',(0.,1.,0.));
#20491=DIRECTION('',(0.,0.892035109009925,-0.45196610967378));
#20492=DIRECTION('center_axis',(0.,-0.45196610967378,-0.892035109009925));
#20493=DIRECTION('ref_axis',(0.,0.892035109009925,-0.45196610967378));
#20494=DIRECTION('',(1.,0.,0.));
#20495=DIRECTION('',(0.,0.892035109009925,-0.45196610967378));
#20496=DIRECTION('center_axis',(1.,0.,0.));
#20497=DIRECTION('ref_axis',(0.,0.17364817766693,-0.984807753012208));
#20498=DIRECTION('center_axis',(1.,0.,0.));
#20499=DIRECTION('ref_axis',(0.,1.,0.));
#20500=DIRECTION('center_axis',(0.,-0.6,0.8));
#20501=DIRECTION('ref_axis',(0.,-0.8,-0.6));
#20502=DIRECTION('',(-1.,0.,0.));
#20503=DIRECTION('',(0.,-0.8,-0.6));
#20504=DIRECTION('',(1.,0.,0.));
#20505=DIRECTION('',(0.,-0.8,-0.6));
#20506=DIRECTION('center_axis',(1.,0.,0.));
#20507=DIRECTION('ref_axis',(0.,0.,-1.));
#20508=DIRECTION('center_axis',(-1.,0.,0.));
#20509=DIRECTION('ref_axis',(0.,1.,0.));
#20510=DIRECTION('',(0.,0.8,-0.6));
#20511=DIRECTION('center_axis',(0.,-0.6,-0.8));
#20512=DIRECTION('ref_axis',(0.,0.8,-0.6));
#20513=DIRECTION('',(1.,0.,0.));
#20514=DIRECTION('',(0.,0.8,-0.6));
#20515=DIRECTION('center_axis',(1.,0.,0.));
#20516=DIRECTION('ref_axis',(0.,0.,-1.));
#20517=DIRECTION('center_axis',(1.,0.,0.));
#20518=DIRECTION('ref_axis',(0.,1.,0.));
#20519=DIRECTION('center_axis',(0.,0.5,0.866025403784439));
#20520=DIRECTION('ref_axis',(0.,0.866025403784439,-0.5));
#20521=DIRECTION('',(0.,0.866025403784439,-0.5));
#20522=DIRECTION('',(-1.,0.,0.));
#20523=DIRECTION('',(0.,0.866025403784439,-0.5));
#20524=DIRECTION('',(-1.,0.,0.));
#20525=DIRECTION('center_axis',(0.,-0.5,0.866025403784439));
#20526=DIRECTION('ref_axis',(0.,0.866025403784439,0.5));
#20527=DIRECTION('',(0.,0.866025403784439,0.5));
#20528=DIRECTION('',(-1.,0.,0.));
#20529=DIRECTION('',(0.,0.866025403784439,0.5));
#20530=DIRECTION('center_axis',(0.,-1.,-1.92296268638356E-16));
#20531=DIRECTION('ref_axis',(0.,-1.92296268638356E-16,1.));
#20532=DIRECTION('',(0.,-1.92296268638356E-16,1.));
#20533=DIRECTION('',(-1.,0.,0.));
#20534=DIRECTION('',(0.,-1.92296268638356E-16,1.));
#20535=DIRECTION('center_axis',(0.,-0.5,-0.866025403784439));
#20536=DIRECTION('ref_axis',(0.,-0.866025403784439,0.5));
#20537=DIRECTION('',(0.,-0.866025403784439,0.5));
#20538=DIRECTION('',(-1.,0.,0.));
#20539=DIRECTION('',(0.,-0.866025403784439,0.5));
#20540=DIRECTION('center_axis',(0.,0.5,-0.866025403784439));
#20541=DIRECTION('ref_axis',(0.,-0.866025403784439,-0.5));
#20542=DIRECTION('',(0.,-0.866025403784439,-0.5));
#20543=DIRECTION('',(-1.,0.,0.));
#20544=DIRECTION('',(0.,-0.866025403784439,-0.5));
#20545=DIRECTION('center_axis',(0.,1.,-3.84592537276713E-16));
#20546=DIRECTION('ref_axis',(0.,-3.84592537276713E-16,-1.));
#20547=DIRECTION('',(0.,-3.84592537276713E-16,-1.));
#20548=DIRECTION('',(0.,-3.84592537276713E-16,-1.));
#20549=DIRECTION('center_axis',(-1.,0.,0.));
#20550=DIRECTION('ref_axis',(0.,0.,1.));
#20551=DIRECTION('center_axis',(-1.,0.,0.));
#20552=DIRECTION('ref_axis',(0.,0.,1.));
#20553=DIRECTION('center_axis',(1.,0.,0.));
#20554=DIRECTION('ref_axis',(0.,0.,-1.));
#20555=DIRECTION('center_axis',(1.,0.,0.));
#20556=DIRECTION('ref_axis',(0.,1.,0.));
#20557=DIRECTION('',(-0.707106781186547,0.707106781186548,8.65956056235494E-17));
#20558=DIRECTION('center_axis',(1.,0.,0.));
#20559=DIRECTION('ref_axis',(0.,1.,0.));
#20560=DIRECTION('center_axis',(1.,0.,0.));
#20561=DIRECTION('ref_axis',(0.,1.,0.));
#20562=DIRECTION('center_axis',(-1.,0.,0.));
#20563=DIRECTION('ref_axis',(0.,0.,1.));
#20564=DIRECTION('center_axis',(1.,0.,0.));
#20565=DIRECTION('ref_axis',(0.,0.,-1.));
#20566=DIRECTION('center_axis',(1.,0.,0.));
#20567=DIRECTION('ref_axis',(0.,1.,0.));
#20568=DIRECTION('center_axis',(1.,0.,0.));
#20569=DIRECTION('ref_axis',(0.,0.,-1.));
#20570=DIRECTION('',(-1.,0.,0.));
#20571=DIRECTION('',(-1.,0.,0.));
#20572=DIRECTION('center_axis',(-1.,0.,0.));
#20573=DIRECTION('ref_axis',(0.,1.,0.));
#20574=DIRECTION('center_axis',(1.,0.,0.));
#20575=DIRECTION('ref_axis',(0.,0.,-1.));
#20576=DIRECTION('',(-0.707106781186547,-0.707106781186548,-8.65956056235494E-17));
#20577=DIRECTION('center_axis',(1.,0.,0.));
#20578=DIRECTION('ref_axis',(0.,0.,-1.));
#20579=DIRECTION('axis',(0.,0.,1.));
#20580=DIRECTION('refdir',(1.,0.,0.));
#20581=DIRECTION('center_axis',(1.,0.,0.));
#20582=DIRECTION('ref_axis',(0.,1.,0.));
#20583=DIRECTION('',(-1.,0.,0.));
#20584=DIRECTION('center_axis',(1.,0.,0.));
#20585=DIRECTION('ref_axis',(0.,1.,0.));
#20586=DIRECTION('center_axis',(1.,0.,0.));
#20587=DIRECTION('ref_axis',(0.,1.,0.));
#20588=DIRECTION('',(-1.,0.,0.));
#20589=DIRECTION('center_axis',(1.,0.,0.));
#20590=DIRECTION('ref_axis',(0.,1.,0.));
#20591=DIRECTION('',(-1.,0.,0.));
#20592=DIRECTION('center_axis',(1.,0.,0.));
#20593=DIRECTION('ref_axis',(0.,1.,0.));
#20594=DIRECTION('',(-1.,0.,0.));
#20595=DIRECTION('center_axis',(1.,0.,0.));
#20596=DIRECTION('ref_axis',(0.,1.,0.));
#20597=DIRECTION('',(-1.,0.,0.));
#20598=DIRECTION('center_axis',(1.,0.,0.));
#20599=DIRECTION('ref_axis',(0.,1.,0.));
#20600=DIRECTION('',(-1.,0.,0.));
#20601=DIRECTION('center_axis',(1.,0.,0.));
#20602=DIRECTION('ref_axis',(0.,1.,0.));
#20603=DIRECTION('',(-1.,0.,0.));
#20604=DIRECTION('center_axis',(1.,0.,0.));
#20605=DIRECTION('ref_axis',(0.,1.,1.99201639031977E-14));
#20606=DIRECTION('',(1.,0.,0.));
#20607=DIRECTION('center_axis',(1.,0.,0.));
#20608=DIRECTION('ref_axis',(0.,1.,1.99201639031977E-14));
#20609=DIRECTION('center_axis',(1.,0.,0.));
#20610=DIRECTION('ref_axis',(0.,1.,1.99201639031977E-14));
#20611=DIRECTION('',(1.,0.,0.));
#20612=DIRECTION('center_axis',(1.,0.,0.));
#20613=DIRECTION('ref_axis',(0.,1.,1.99201639031977E-14));
#20614=DIRECTION('center_axis',(1.,0.,0.));
#20615=DIRECTION('ref_axis',(0.,1.,1.99201639031977E-14));
#20616=DIRECTION('',(1.,0.,0.));
#20617=DIRECTION('center_axis',(1.,0.,0.));
#20618=DIRECTION('ref_axis',(0.,1.,1.99201639031977E-14));
#20619=DIRECTION('',(1.,0.,0.));
#20620=DIRECTION('center_axis',(1.,0.,0.));
#20621=DIRECTION('ref_axis',(0.,1.,1.99201639031977E-14));
#20622=DIRECTION('',(1.,0.,0.));
#20623=DIRECTION('center_axis',(1.,0.,0.));
#20624=DIRECTION('ref_axis',(0.,1.,1.99201639031977E-14));
#20625=DIRECTION('',(1.,0.,0.));
#20626=DIRECTION('center_axis',(1.,0.,0.));
#20627=DIRECTION('ref_axis',(0.,1.,1.99201639031977E-14));
#20628=DIRECTION('',(1.,0.,0.));
#20629=DIRECTION('center_axis',(0.547750005235851,-0.72455327535185,0.418321028566616));
#20630=DIRECTION('ref_axis',(0.606949534647157,0.,-0.79474037420506));
#20631=DIRECTION('',(0.67749794402081,0.0907675134870617,-0.729902592366236));
#20632=DIRECTION('',(0.,0.5,0.866025403784439));
#20633=DIRECTION('',(-0.677497944020809,-0.677497944020809,-0.286344323664976));
#20634=DIRECTION('center_axis',(0.,-0.866025403784439,0.5));
#20635=DIRECTION('ref_axis',(1.,0.,0.));
#20636=DIRECTION('',(0.,0.5,0.866025403784439));
#20637=DIRECTION('',(1.,0.,0.));
#20638=DIRECTION('',(-1.,0.,0.));
#20639=DIRECTION('center_axis',(0.547750005235851,0.,0.836642057133232));
#20640=DIRECTION('ref_axis',(0.836642057133232,0.,-0.547750005235851));
#20641=DIRECTION('',(0.677497944020809,-0.586730430533747,-0.443558268701262));
#20642=DIRECTION('',(0.,1.,0.));
#20643=DIRECTION('',(-0.67749794402081,-0.586730430533748,0.44355826870126));
#20644=DIRECTION('center_axis',(0.,0.,1.));
#20645=DIRECTION('ref_axis',(1.,0.,0.));
#20646=DIRECTION('',(0.,1.,0.));
#20647=DIRECTION('',(1.,0.,0.));
#20648=DIRECTION('',(-1.,0.,0.));
#20649=DIRECTION('center_axis',(0.707106781186547,-0.353553390593274,0.612372435695795));
#20650=DIRECTION('ref_axis',(0.654653670707978,0.,-0.755928946018454));
#20651=DIRECTION('',(0.,0.866025403784439,0.5));
#20652=DIRECTION('',(0.,-0.866025403784439,-0.5));
#20653=DIRECTION('center_axis',(0.547750005235851,-0.72455327535185,-0.418321028566615));
#20654=DIRECTION('ref_axis',(-0.606949534647157,0.,-0.79474037420506));
#20655=DIRECTION('',(0.677497944020809,0.677497944020809,-0.286344323664979));
#20656=DIRECTION('',(0.,-0.499999999999999,0.866025403784439));
#20657=DIRECTION('',(-0.67749794402081,-0.0907675134870617,-0.729902592366236));
#20658=DIRECTION('center_axis',(0.,-0.866025403784439,-0.5));
#20659=DIRECTION('ref_axis',(0.,0.5,-0.866025403784439));
#20660=DIRECTION('',(0.,-0.5,0.866025403784439));
#20661=DIRECTION('',(1.,0.,0.));
#20662=DIRECTION('',(-1.,0.,0.));
#20663=DIRECTION('center_axis',(0.547750005235849,0.724553275351851,0.418321028566616));
#20664=DIRECTION('ref_axis',(0.606949534647159,0.,-0.794740374205059));
#20665=DIRECTION('',(0.677497944020811,-0.677497944020808,0.286344323664977));
#20666=DIRECTION('',(0.,0.499999999999999,-0.866025403784439));
#20667=DIRECTION('',(-0.677497944020809,0.0907675134870586,0.729902592366237));
#20668=DIRECTION('center_axis',(0.,0.866025403784439,0.5));
#20669=DIRECTION('ref_axis',(0.,-0.5,0.866025403784439));
#20670=DIRECTION('',(0.,0.5,-0.866025403784439));
#20671=DIRECTION('',(1.,0.,0.));
#20672=DIRECTION('',(-1.,0.,0.));
#20673=DIRECTION('center_axis',(0.707106781186547,0.353553390593274,0.612372435695795));
#20674=DIRECTION('ref_axis',(0.654653670707978,0.,-0.755928946018454));
#20675=DIRECTION('',(0.,0.866025403784439,-0.5));
#20676=DIRECTION('',(0.,-0.866025403784439,0.5));
#20677=DIRECTION('center_axis',(0.547750005235851,0.,-0.836642057133232));
#20678=DIRECTION('ref_axis',(-0.836642057133232,0.,-0.547750005235851));
#20679=DIRECTION('',(0.67749794402081,0.586730430533747,0.44355826870126));
#20680=DIRECTION('',(0.,-1.,0.));
#20681=DIRECTION('',(-0.67749794402081,0.586730430533747,-0.44355826870126));
#20682=DIRECTION('center_axis',(0.,0.,-1.));
#20683=DIRECTION('ref_axis',(-1.,0.,0.));
#20684=DIRECTION('',(0.,-1.,0.));
#20685=DIRECTION('',(1.,0.,0.));
#20686=DIRECTION('',(-1.,0.,0.));
#20687=DIRECTION('center_axis',(0.547750005235848,0.724553275351853,-0.418321028566616));
#20688=DIRECTION('ref_axis',(-0.60694953464716,0.,-0.794740374205058));
#20689=DIRECTION('',(0.67749794402081,-0.0907675134870617,0.729902592366236));
#20690=DIRECTION('',(0.,-0.499999999999999,-0.866025403784439));
#20691=DIRECTION('',(-0.67749794402081,0.677497944020807,0.286344323664981));
#20692=DIRECTION('center_axis',(0.,0.866025403784439,-0.499999999999999));
#20693=DIRECTION('ref_axis',(0.,0.499999999999999,0.866025403784439));
#20694=DIRECTION('',(0.,-0.499999999999999,-0.866025403784439));
#20695=DIRECTION('',(1.,0.,0.));
#20696=DIRECTION('',(-1.,0.,0.));
#20697=DIRECTION('center_axis',(0.707106781186546,0.707106781186549,-2.47225446456458E-16));
#20698=DIRECTION('ref_axis',(-3.49629579342468E-16,0.,-1.));
#20699=DIRECTION('',(0.,-3.49629579342466E-16,-1.));
#20700=DIRECTION('',(0.,3.49629579342466E-16,1.));
#20701=DIRECTION('center_axis',(0.707106781186547,0.353553390593274,-0.612372435695795));
#20702=DIRECTION('ref_axis',(-0.654653670707978,0.,-0.755928946018454));
#20703=DIRECTION('',(0.,-0.866025403784439,-0.5));
#20704=DIRECTION('',(0.,0.866025403784439,0.5));
#20705=DIRECTION('center_axis',(0.707106781186547,-0.353553390593274,-0.612372435695795));
#20706=DIRECTION('ref_axis',(-0.654653670707978,0.,-0.755928946018454));
#20707=DIRECTION('',(0.,-0.866025403784439,0.5));
#20708=DIRECTION('',(0.,0.866025403784439,-0.5));
#20709=DIRECTION('center_axis',(0.707106781186548,-0.707106781186548,0.));
#20710=DIRECTION('ref_axis',(0.,0.,-1.));
#20711=DIRECTION('',(0.,0.,1.));
#20712=DIRECTION('',(0.,0.,-1.));
#20713=DIRECTION('center_axis',(0.,-0.5,0.866025403784439));
#20714=DIRECTION('ref_axis',(0.,-0.866025403784439,-0.5));
#20715=DIRECTION('',(0.,0.866025403784439,0.5));
#20716=DIRECTION('center_axis',(0.,0.5,0.866025403784439));
#20717=DIRECTION('ref_axis',(0.,-0.866025403784439,0.5));
#20718=DIRECTION('',(0.,0.866025403784439,-0.5));
#20719=DIRECTION('center_axis',(0.,1.,-3.49629579342466E-16));
#20720=DIRECTION('ref_axis',(0.,3.49629579342466E-16,1.));
#20721=DIRECTION('',(0.,-3.49629579342466E-16,-1.));
#20722=DIRECTION('center_axis',(1.,0.,0.));
#20723=DIRECTION('ref_axis',(0.,0.,-1.));
#20724=DIRECTION('',(0.,-0.866025403784439,0.5));
#20725=DIRECTION('',(0.,3.60555503696918E-16,1.));
#20726=DIRECTION('',(0.,0.866025403784439,0.5));
#20727=DIRECTION('',(0.,0.866025403784439,-0.5));
#20728=DIRECTION('',(0.,1.20185167898973E-16,-1.));
#20729=DIRECTION('',(0.,-0.866025403784439,-0.5));
#20730=DIRECTION('center_axis',(0.707106781186548,0.353553390593274,0.612372435695794));
#20731=DIRECTION('ref_axis',(0.654653670707977,0.,-0.755928946018455));
#20732=DIRECTION('',(-0.654653670707977,3.42727999801544E-16,0.755928946018454));
#20733=DIRECTION('',(0.,-0.866025403784439,0.5));
#20734=DIRECTION('',(-0.654653670707977,0.654653670707977,0.377964473009228));
#20735=DIRECTION('center_axis',(0.707106781186548,-0.353553390593274,0.612372435695795));
#20736=DIRECTION('ref_axis',(0.654653670707977,0.,-0.755928946018454));
#20737=DIRECTION('',(-0.654653670707977,-0.654653670707976,0.377964473009229));
#20738=DIRECTION('',(0.,-0.866025403784439,-0.5));
#20739=DIRECTION('center_axis',(0.707106781186547,-0.353553390593274,-0.612372435695795));
#20740=DIRECTION('ref_axis',(-0.654653670707978,0.,-0.755928946018454));
#20741=DIRECTION('',(-0.654653670707977,3.70298385649733E-16,-0.755928946018454));
#20742=DIRECTION('',(0.,0.866025403784439,-0.5));
#20743=DIRECTION('',(0.654653670707978,0.654653670707977,0.377964473009227));
#20744=DIRECTION('center_axis',(0.707106781186548,0.353553390593274,-0.612372435695794));
#20745=DIRECTION('ref_axis',(-0.654653670707977,0.,-0.755928946018455));
#20746=DIRECTION('',(0.,0.866025403784439,0.5));
#20747=DIRECTION('',(-0.654653670707977,0.654653670707977,-0.377964473009228));
#20748=DIRECTION('center_axis',(0.707106781186547,-0.707106781186548,2.54951241658222E-16));
#20749=DIRECTION('ref_axis',(3.60555503696919E-16,0.,-1.));
#20750=DIRECTION('',(0.,-3.60555503696918E-16,-1.));
#20751=DIRECTION('center_axis',(0.707106781186548,0.707106781186548,8.49837472194074E-17));
#20752=DIRECTION('ref_axis',(1.20185167898973E-16,0.,-1.));
#20753=DIRECTION('',(0.,-1.20185167898973E-16,1.));
#20754=DIRECTION('center_axis',(0.,0.5,-0.866025403784439));
#20755=DIRECTION('ref_axis',(0.,-0.866025403784439,-0.5));
#20756=DIRECTION('',(-1.,0.,0.));
#20757=DIRECTION('',(0.,-0.866025403784439,-0.5));
#20758=DIRECTION('',(-1.,0.,0.));
#20759=DIRECTION('center_axis',(0.,1.,-3.60555503696918E-16));
#20760=DIRECTION('ref_axis',(0.,-3.60555503696918E-16,-1.));
#20761=DIRECTION('',(-1.,0.,0.));
#20762=DIRECTION('',(0.,-3.60555503696918E-16,-1.));
#20763=DIRECTION('center_axis',(0.,0.5,0.866025403784439));
#20764=DIRECTION('ref_axis',(0.,0.866025403784439,-0.5));
#20765=DIRECTION('',(-1.,0.,0.));
#20766=DIRECTION('',(0.,0.866025403784439,-0.5));
#20767=DIRECTION('center_axis',(1.,0.,0.));
#20768=DIRECTION('ref_axis',(0.,0.,-1.));
#20769=DIRECTION('center_axis',(1.,0.,0.));
#20770=DIRECTION('ref_axis',(0.,1.,0.));
#20771=DIRECTION('center_axis',(1.,0.,0.));
#20772=DIRECTION('ref_axis',(0.,1.,0.));
#20773=DIRECTION('center_axis',(-1.,0.,0.));
#20774=DIRECTION('ref_axis',(0.,1.,1.99201639031977E-14));
#20775=DIRECTION('center_axis',(1.,0.,0.));
#20776=DIRECTION('ref_axis',(0.,1.,1.99201639031977E-14));
#20777=DIRECTION('center_axis',(1.,0.,0.));
#20778=DIRECTION('ref_axis',(0.,0.,-1.));
#20779=DIRECTION('center_axis',(-1.,0.,0.));
#20780=DIRECTION('ref_axis',(0.,1.,0.));
#20781=DIRECTION('center_axis',(1.,0.,0.));
#20782=DIRECTION('ref_axis',(0.,0.,-1.));
#20783=DIRECTION('center_axis',(0.,-0.5,0.866025403784439));
#20784=DIRECTION('ref_axis',(0.,0.866025403784439,0.5));
#20785=DIRECTION('',(-1.,0.,0.));
#20786=DIRECTION('',(0.,0.866025403784439,0.5));
#20787=DIRECTION('center_axis',(0.,-1.,-1.20185167898973E-16));
#20788=DIRECTION('ref_axis',(0.,-1.20185167898973E-16,1.));
#20789=DIRECTION('',(-1.,0.,0.));
#20790=DIRECTION('',(0.,-1.20185167898973E-16,1.));
#20791=DIRECTION('center_axis',(0.,-0.5,-0.866025403784439));
#20792=DIRECTION('ref_axis',(0.,-0.866025403784439,0.5));
#20793=DIRECTION('',(0.,-0.866025403784439,0.5));
#20794=DIRECTION('center_axis',(-1.,0.,0.));
#20795=DIRECTION('ref_axis',(0.,0.,1.));
#20796=DIRECTION('center_axis',(0.,0.5,-0.866025403784439));
#20797=DIRECTION('ref_axis',(0.,0.866025403784439,0.5));
#20798=DIRECTION('',(0.,-0.866025403784439,-0.5));
#20799=DIRECTION('center_axis',(0.,-0.5,-0.866025403784439));
#20800=DIRECTION('ref_axis',(0.,0.866025403784439,-0.5));
#20801=DIRECTION('',(0.,-0.866025403784439,0.5));
#20802=DIRECTION('center_axis',(0.,-1.,0.));
#20803=DIRECTION('ref_axis',(0.,0.,-1.));
#20804=DIRECTION('',(0.,0.,1.));
#20805=DIRECTION('center_axis',(1.,0.,0.));
#20806=DIRECTION('ref_axis',(0.,0.,-1.));
#20807=DIRECTION('center_axis',(1.,0.,0.));
#20808=DIRECTION('ref_axis',(0.,0.,-1.));
#20809=DIRECTION('center_axis',(-1.,0.,0.));
#20810=DIRECTION('ref_axis',(0.,0.,1.));
#20811=DIRECTION('center_axis',(1.,0.,0.));
#20812=DIRECTION('ref_axis',(0.,0.,-1.));
#20813=DIRECTION('center_axis',(1.,0.,0.));
#20814=DIRECTION('ref_axis',(0.,0.,-1.));
#20815=DIRECTION('center_axis',(1.,0.,0.));
#20816=DIRECTION('ref_axis',(0.,1.,0.));
#20817=DIRECTION('',(-1.,0.,0.));
#20818=DIRECTION('center_axis',(-1.,0.,0.));
#20819=DIRECTION('ref_axis',(0.,0.,1.));
#20820=DIRECTION('center_axis',(1.,0.,0.));
#20821=DIRECTION('ref_axis',(0.,0.,-1.));
#20822=DIRECTION('center_axis',(1.,0.,0.));
#20823=DIRECTION('ref_axis',(0.,1.,0.));
#20824=DIRECTION('',(-0.707106781186547,0.707106781186548,8.65956056235494E-17));
#20825=DIRECTION('center_axis',(1.,0.,0.));
#20826=DIRECTION('ref_axis',(0.,1.,0.));
#20827=DIRECTION('center_axis',(1.,0.,0.));
#20828=DIRECTION('ref_axis',(0.,1.,0.));
#20829=DIRECTION('',(-1.,0.,0.));
#20830=DIRECTION('',(0.,0.,1.));
#20831=DIRECTION('',(1.,0.,0.));
#20832=DIRECTION('',(0.,0.,1.));
#20833=DIRECTION('',(1.,0.,0.));
#20834=DIRECTION('',(0.,0.,1.));
#20835=DIRECTION('',(1.,0.,0.));
#20836=DIRECTION('',(0.,0.,1.));
#20837=DIRECTION('',(1.,0.,0.));
#20838=DIRECTION('',(0.,0.,1.));
#20839=DIRECTION('',(1.,0.,0.));
#20840=DIRECTION('',(0.,0.,1.));
#20841=DIRECTION('',(1.,0.,0.));
#20842=DIRECTION('',(0.,0.,1.));
#20843=DIRECTION('',(1.,0.,0.));
#20844=DIRECTION('',(0.,0.,1.));
#20845=DIRECTION('',(1.,0.,0.));
#20846=DIRECTION('',(0.,0.,1.));
#20847=DIRECTION('',(1.,0.,0.));
#20848=DIRECTION('',(0.,0.,1.));
#20849=DIRECTION('',(1.,0.,0.));
#20850=DIRECTION('',(0.,0.,1.));
#20851=DIRECTION('',(1.,0.,0.));
#20852=DIRECTION('',(-0.309016994374947,0.,0.951056516295153));
#20853=DIRECTION('',(0.951056516295154,0.,0.309016994374947));
#20854=DIRECTION('',(0.,0.,1.));
#20855=DIRECTION('',(1.,0.,0.));
#20856=DIRECTION('',(-0.309016994374947,0.,0.951056516295153));
#20857=DIRECTION('',(0.951056516295154,0.,0.309016994374947));
#20858=DIRECTION('',(0.,0.,1.));
#20859=DIRECTION('',(1.,0.,0.));
#20860=DIRECTION('',(-0.309016994374947,0.,0.951056516295153));
#20861=DIRECTION('',(0.951056516295154,0.,0.309016994374947));
#20862=DIRECTION('',(0.,0.,1.));
#20863=DIRECTION('',(1.,0.,0.));
#20864=DIRECTION('',(-0.309016994374947,0.,0.951056516295153));
#20865=DIRECTION('',(0.951056516295154,0.,0.309016994374947));
#20866=DIRECTION('',(0.,0.,1.));
#20867=DIRECTION('',(1.,0.,0.));
#20868=DIRECTION('',(-0.309016994374947,0.,0.951056516295153));
#20869=DIRECTION('',(0.951056516295154,0.,0.309016994374947));
#20870=DIRECTION('',(0.,0.,1.));
#20871=DIRECTION('',(1.,0.,0.));
#20872=DIRECTION('',(-0.309016994374947,0.,0.951056516295153));
#20873=DIRECTION('',(0.951056516295154,0.,0.309016994374947));
#20874=DIRECTION('',(0.,0.,1.));
#20875=DIRECTION('',(1.,0.,0.));
#20876=DIRECTION('',(-0.309016994374947,0.,0.951056516295153));
#20877=DIRECTION('',(0.951056516295154,0.,0.309016994374947));
#20878=DIRECTION('',(-0.309016994374947,0.,0.951056516295154));
#20879=DIRECTION('',(0.951056516295154,0.,0.309016994374947));
#20880=DIRECTION('',(0.,0.,1.));
#20881=DIRECTION('',(1.,0.,0.));
#20882=DIRECTION('',(0.,0.,1.));
#20883=DIRECTION('',(1.,0.,0.));
#20884=DIRECTION('',(0.,0.,1.));
#20885=DIRECTION('',(1.,0.,0.));
#20886=DIRECTION('',(0.,0.,1.));
#20887=DIRECTION('',(1.,0.,0.));
#20888=DIRECTION('',(0.,-1.,0.));
#20889=DIRECTION('',(0.,0.,-1.));
#20890=CARTESIAN_POINT('',(0.,0.,0.));
#20891=CARTESIAN_POINT('',(0.,0.,0.));
#20892=CARTESIAN_POINT('Origin',(62.5,18.,-63.75));
#20893=CARTESIAN_POINT('',(48.,18.,-64.));
#20894=CARTESIAN_POINT('Origin',(62.5,18.,-64.));
#20895=CARTESIAN_POINT('',(47.5,18.,-63.5));
#20896=CARTESIAN_POINT('',(47.75,18.,-63.75));
#20897=CARTESIAN_POINT('Origin',(62.5,18.,-63.5));
#20898=CARTESIAN_POINT('Origin',(62.5,18.,-50.));
#20899=CARTESIAN_POINT('',(47.5,18.,-60.));
#20900=CARTESIAN_POINT('',(47.5,18.,-50.));
#20901=CARTESIAN_POINT('',(57.1148351928655,32.,-60.));
#20902=CARTESIAN_POINT('Origin',(62.5,18.,-60.));
#20903=CARTESIAN_POINT('',(67.8851648071345,32.,-60.));
#20904=CARTESIAN_POINT('Ctrl Pts',(67.8851648071345,32.,-60.));
#20905=CARTESIAN_POINT('Ctrl Pts',(67.6984748326239,32.0718111628985,-60.));
#20906=CARTESIAN_POINT('Ctrl Pts',(67.5101785201311,32.1399502129255,-59.9997241719152));
#20907=CARTESIAN_POINT('Ctrl Pts',(65.73704131346,32.7417106379464,-59.9953335785546));
#20908=CARTESIAN_POINT('Ctrl Pts',(64.0583526295515,33.,-59.9821371592664));
#20909=CARTESIAN_POINT('Ctrl Pts',(60.9416473704485,33.,-59.9821371592664));
#20910=CARTESIAN_POINT('Ctrl Pts',(59.26295868654,32.7417106379464,-59.9953335785546));
#20911=CARTESIAN_POINT('Ctrl Pts',(57.4898214798689,32.1399502129255,-59.9997241719152));
#20912=CARTESIAN_POINT('Ctrl Pts',(57.3015251673761,32.0718111628985,-60.));
#20913=CARTESIAN_POINT('Ctrl Pts',(57.1148351928655,32.,-60.));
#20914=CARTESIAN_POINT('Origin',(62.5,18.,-60.));
#20915=CARTESIAN_POINT('Origin',(62.5,18.,-64.));
#20916=CARTESIAN_POINT('',(53.45,18.,-64.));
#20917=CARTESIAN_POINT('Origin',(62.5,18.,-64.));
#20918=CARTESIAN_POINT('Origin',(15.75,-73.,0.));
#20919=CARTESIAN_POINT('',(16.,-73.,7.65));
#20920=CARTESIAN_POINT('Origin',(16.,-73.,0.));
#20921=CARTESIAN_POINT('',(15.5,-73.,7.15));
#20922=CARTESIAN_POINT('',(15.75,-73.,7.4));
#20923=CARTESIAN_POINT('Origin',(15.5,-73.,0.));
#20924=CARTESIAN_POINT('Origin',(16.,0.,0.));
#20925=CARTESIAN_POINT('',(16.,-60.8276253029822,-12.));
#20926=CARTESIAN_POINT('',(16.,-73.,-12.));
#20927=CARTESIAN_POINT('',(16.,-36.5,-12.));
#20928=CARTESIAN_POINT('',(16.,-60.,-15.6204993518133));
#20929=CARTESIAN_POINT('Origin',(16.,0.,0.));
#20930=CARTESIAN_POINT('',(16.,-60.,15.6204993518133));
#20931=CARTESIAN_POINT('',(16.,-60.,16.));
#20932=CARTESIAN_POINT('',(16.,-60.8276253029822,12.));
#20933=CARTESIAN_POINT('Origin',(16.,0.,0.));
#20934=CARTESIAN_POINT('',(16.,-73.,12.));
#20935=CARTESIAN_POINT('',(16.,-30.4559107563704,12.));
#20936=CARTESIAN_POINT('Origin',(16.,-73.,0.));
#20937=CARTESIAN_POINT('Origin',(-0.1,-73.,0.));
#20938=CARTESIAN_POINT('',(0.5,-73.,7.15));
#20939=CARTESIAN_POINT('Origin',(0.5,-73.,0.));
#20940=CARTESIAN_POINT('',(-0.1,-73.,7.15));
#20941=CARTESIAN_POINT('Origin',(62.5,18.,63.75));
#20942=CARTESIAN_POINT('',(48.,18.,64.));
#20943=CARTESIAN_POINT('Origin',(62.5,18.,64.));
#20944=CARTESIAN_POINT('',(47.5,18.,63.5));
#20945=CARTESIAN_POINT('',(47.75,18.,63.75));
#20946=CARTESIAN_POINT('Origin',(62.5,18.,63.5));
#20947=CARTESIAN_POINT('Origin',(62.5,18.,64.));
#20948=CARTESIAN_POINT('',(52.95,18.,64.));
#20949=CARTESIAN_POINT('Origin',(62.5,18.,64.));
#20950=CARTESIAN_POINT('Origin',(62.5,18.,50.));
#20951=CARTESIAN_POINT('',(47.5,18.,60.));
#20952=CARTESIAN_POINT('',(47.5,18.,50.));
#20953=CARTESIAN_POINT('',(67.8851648071345,32.,60.));
#20954=CARTESIAN_POINT('Origin',(62.5,18.,60.));
#20955=CARTESIAN_POINT('',(57.1148351928655,32.,60.));
#20956=CARTESIAN_POINT('Ctrl Pts',(57.1148351928655,32.,60.));
#20957=CARTESIAN_POINT('Ctrl Pts',(57.3015251673761,32.0718111628985,60.));
#20958=CARTESIAN_POINT('Ctrl Pts',(57.4898214798689,32.1399502129255,59.9997241719152));
#20959=CARTESIAN_POINT('Ctrl Pts',(59.26295868654,32.7417106379464,59.9953335785546));
#20960=CARTESIAN_POINT('Ctrl Pts',(60.9416473704485,33.,59.9821371592664));
#20961=CARTESIAN_POINT('Ctrl Pts',(64.0583526295515,33.,59.9821371592664));
#20962=CARTESIAN_POINT('Ctrl Pts',(65.73704131346,32.7417106379464,59.9953335785546));
#20963=CARTESIAN_POINT('Ctrl Pts',(67.5101785201311,32.1399502129255,59.9997241719152));
#20964=CARTESIAN_POINT('Ctrl Pts',(67.6984748326239,32.0718111628985,60.));
#20965=CARTESIAN_POINT('Ctrl Pts',(67.8851648071345,32.,60.));
#20966=CARTESIAN_POINT('Origin',(62.5,18.,60.));
#20967=CARTESIAN_POINT('Origin',(15.75,73.,0.));
#20968=CARTESIAN_POINT('',(16.,73.,7.65));
#20969=CARTESIAN_POINT('Origin',(16.,73.,0.));
#20970=CARTESIAN_POINT('',(15.5,73.,7.15));
#20971=CARTESIAN_POINT('',(15.75,73.,7.4));
#20972=CARTESIAN_POINT('Origin',(15.5,73.,0.));
#20973=CARTESIAN_POINT('Origin',(16.,0.,0.));
#20974=CARTESIAN_POINT('',(16.,73.,-12.));
#20975=CARTESIAN_POINT('',(16.,60.8276253029822,-12.));
#20976=CARTESIAN_POINT('',(16.,30.4559107563704,-12.));
#20977=CARTESIAN_POINT('',(16.,73.,12.));
#20978=CARTESIAN_POINT('Origin',(16.,73.,0.));
#20979=CARTESIAN_POINT('',(16.,60.8276253029822,12.));
#20980=CARTESIAN_POINT('',(16.,36.5,12.));
#20981=CARTESIAN_POINT('',(16.,60.,15.6204993518133));
#20982=CARTESIAN_POINT('Origin',(16.,0.,0.));
#20983=CARTESIAN_POINT('',(16.,60.,-15.6204993518133));
#20984=CARTESIAN_POINT('',(16.,60.,-16.));
#20985=CARTESIAN_POINT('Origin',(16.,0.,0.));
#20986=CARTESIAN_POINT('Origin',(-0.1,73.,0.));
#20987=CARTESIAN_POINT('',(0.5,73.,7.15));
#20988=CARTESIAN_POINT('Origin',(0.5,73.,0.));
#20989=CARTESIAN_POINT('',(-0.1,73.,7.15));
#20990=CARTESIAN_POINT('Origin',(62.5,18.,63.75));
#20991=CARTESIAN_POINT('',(53.45,18.,63.5));
#20992=CARTESIAN_POINT('',(53.2,18.,63.75));
#20993=CARTESIAN_POINT('Origin',(62.5,18.,63.5));
#20994=CARTESIAN_POINT('Origin',(62.5,18.,64.));
#20995=CARTESIAN_POINT('',(53.44935360134,18.0005320189151,48.7866812026286));
#20996=CARTESIAN_POINT('',(53.45,18.,64.));
#20997=CARTESIAN_POINT('',(55.0359921611649,23.1177228316711,46.0000000008449));
#20998=CARTESIAN_POINT('Ctrl Pts',(55.0359921613628,23.1177228319597,46.0000000015041));
#20999=CARTESIAN_POINT('Ctrl Pts',(54.0296627121601,21.6500288704652,46.9446698142113));
#21000=CARTESIAN_POINT('Ctrl Pts',(53.4516146271291,19.8715344775383,47.9435639657356));
#21001=CARTESIAN_POINT('Ctrl Pts',(53.4492786369557,18.0256888439599,48.7753807839716));
#21002=CARTESIAN_POINT('Ctrl Pts',(53.44935360134,18.0005320189151,48.7866812026286));
#21003=CARTESIAN_POINT('',(69.9640078370496,23.1177228342753,46.0000000000068));
#21004=CARTESIAN_POINT('Origin',(62.5,18.,46.));
#21005=CARTESIAN_POINT('Ctrl Pts',(53.44935360134,18.0005320189151,48.7866812026286));
#21006=CARTESIAN_POINT('Ctrl Pts',(53.4547065835389,16.2041584743725,49.5936102599095));
#21007=CARTESIAN_POINT('Ctrl Pts',(54.5621164439011,12.4685238830907,50.8988378408999));
#21008=CARTESIAN_POINT('Ctrl Pts',(59.4315484638286,8.79278472652513,51.5632592674646));
#21009=CARTESIAN_POINT('Ctrl Pts',(65.5663223673701,8.80057359018861,51.5646626464224));
#21010=CARTESIAN_POINT('Ctrl Pts',(70.463129301692,12.4814952571317,50.8974409168532));
#21011=CARTESIAN_POINT('Ctrl Pts',(72.1120278968484,18.1410701930242,48.9161444008817));
#21012=CARTESIAN_POINT('Ctrl Pts',(70.9703446072329,21.6500181963829,46.944676684654));
#21013=CARTESIAN_POINT('Ctrl Pts',(69.964007837035,23.1177228342965,46.));
#21014=CARTESIAN_POINT('Origin',(125.55,45.,-45.));
#21015=CARTESIAN_POINT('',(125.8,45.,-38.45));
#21016=CARTESIAN_POINT('Origin',(125.8,45.,-45.));
#21017=CARTESIAN_POINT('',(125.3,45.,-38.95));
#21018=CARTESIAN_POINT('',(125.55,45.,-38.7));
#21019=CARTESIAN_POINT('Origin',(125.3,45.,-45.));
#21020=CARTESIAN_POINT('Origin',(125.8,0.,0.));
#21021=CARTESIAN_POINT('',(125.8,32.,-58.));
#21022=CARTESIAN_POINT('',(125.8,-32.,-58.));
#21023=CARTESIAN_POINT('',(125.8,-16.,-58.));
#21024=CARTESIAN_POINT('',(125.8,58.,-32.));
#21025=CARTESIAN_POINT('Origin',(125.8,32.,-32.));
#21026=CARTESIAN_POINT('',(125.8,58.,32.));
#21027=CARTESIAN_POINT('',(125.8,58.,-16.));
#21028=CARTESIAN_POINT('',(125.8,32.,58.));
#21029=CARTESIAN_POINT('Origin',(125.8,32.,32.));
#21030=CARTESIAN_POINT('',(125.8,-32.,58.));
#21031=CARTESIAN_POINT('',(125.8,16.,58.));
#21032=CARTESIAN_POINT('',(125.8,-58.,32.));
#21033=CARTESIAN_POINT('Origin',(125.8,-32.,32.));
#21034=CARTESIAN_POINT('',(125.8,-58.,-32.));
#21035=CARTESIAN_POINT('',(125.8,-58.,16.));
#21036=CARTESIAN_POINT('Origin',(125.8,-32.,-32.));
#21037=CARTESIAN_POINT('',(125.8,-45.,51.55));
#21038=CARTESIAN_POINT('Origin',(125.8,-45.,45.));
#21039=CARTESIAN_POINT('',(125.8,-45.,-38.45));
#21040=CARTESIAN_POINT('Origin',(125.8,-45.,-45.));
#21041=CARTESIAN_POINT('',(125.8,-6.36816335556624E-15,-52.));
#21042=CARTESIAN_POINT('Origin',(125.8,0.,0.));
#21043=CARTESIAN_POINT('',(125.8,45.,51.55));
#21044=CARTESIAN_POINT('Origin',(125.8,45.,45.));
#21045=CARTESIAN_POINT('Origin',(125.8,45.,-45.));
#21046=CARTESIAN_POINT('',(99.8,45.,-38.95));
#21047=CARTESIAN_POINT('',(125.8,45.,-38.95));
#21048=CARTESIAN_POINT('Origin',(99.8,45.,-45.));
#21049=CARTESIAN_POINT('Origin',(125.55,-45.,45.));
#21050=CARTESIAN_POINT('',(125.3,-45.,51.05));
#21051=CARTESIAN_POINT('',(125.55,-45.,51.3));
#21052=CARTESIAN_POINT('Origin',(125.3,-45.,45.));
#21053=CARTESIAN_POINT('Origin',(125.8,-45.,45.));
#21054=CARTESIAN_POINT('',(99.8,-45.,51.05));
#21055=CARTESIAN_POINT('',(125.8,-45.,51.05));
#21056=CARTESIAN_POINT('Origin',(99.8,-45.,45.));
#21057=CARTESIAN_POINT('Origin',(125.55,45.,45.));
#21058=CARTESIAN_POINT('',(125.3,45.,51.05));
#21059=CARTESIAN_POINT('',(125.55,45.,51.3));
#21060=CARTESIAN_POINT('Origin',(125.3,45.,45.));
#21061=CARTESIAN_POINT('Origin',(125.8,45.,45.));
#21062=CARTESIAN_POINT('',(99.8,45.,51.05));
#21063=CARTESIAN_POINT('',(125.8,45.,51.05));
#21064=CARTESIAN_POINT('Origin',(99.8,45.,45.));
#21065=CARTESIAN_POINT('Origin',(125.55,-45.,-45.));
#21066=CARTESIAN_POINT('',(125.3,-45.,-38.95));
#21067=CARTESIAN_POINT('',(125.55,-45.,-38.7));
#21068=CARTESIAN_POINT('Origin',(125.3,-45.,-45.));
#21069=CARTESIAN_POINT('Origin',(125.8,-45.,-45.));
#21070=CARTESIAN_POINT('',(99.8,-45.,-38.95));
#21071=CARTESIAN_POINT('',(125.8,-45.,-38.95));
#21072=CARTESIAN_POINT('Origin',(99.8,-45.,-45.));
#21073=CARTESIAN_POINT('Origin',(15.75,0.,0.));
#21074=CARTESIAN_POINT('',(15.4999999969433,-61.0634996055951,-13.3228756624643));
#21075=CARTESIAN_POINT('Ctrl Pts',(15.4999999966277,-61.0634996097249,-13.3228756593561));
#21076=CARTESIAN_POINT('Ctrl Pts',(15.5800859964154,-61.0013423773347,-13.2320666717072));
#21077=CARTESIAN_POINT('Ctrl Pts',(15.6534629211121,-60.9478909731446,-13.1321977587055));
#21078=CARTESIAN_POINT('Ctrl Pts',(15.8336779042045,-60.8282401952317,-12.8299273372329));
#21079=CARTESIAN_POINT('Ctrl Pts',(15.9261070025809,-60.7835362526876,-12.5931700844189));
#21080=CARTESIAN_POINT('Ctrl Pts',(15.9898935814354,-60.7916707113854,-12.2327047392017));
#21081=CARTESIAN_POINT('Ctrl Pts',(16.,-60.80493204889,-12.1150313964023));
#21082=CARTESIAN_POINT('Ctrl Pts',(16.,-60.8276253029822,-11.9999999999999));
#21083=CARTESIAN_POINT('',(15.5,-59.8580811200045,-17.9794361599846));
#21084=CARTESIAN_POINT('Origin',(15.5,0.,0.));
#21085=CARTESIAN_POINT('',(15.6381526893245,-60.,-17.));
#21086=CARTESIAN_POINT('Ctrl Pts',(15.5,-59.8580811200045,-17.9794361599846));
#21087=CARTESIAN_POINT('Ctrl Pts',(15.5485606843564,-59.9053376415118,-17.6533009342783));
#21088=CARTESIAN_POINT('Ctrl Pts',(15.5946215988532,-59.9526427924876,-17.3268300981166));
#21089=CARTESIAN_POINT('Ctrl Pts',(15.6381526893245,-60.,-17.));
#21090=CARTESIAN_POINT('Ctrl Pts',(15.6381526893245,-60.,-17.));
#21091=CARTESIAN_POINT('Ctrl Pts',(15.826727493626,-60.,-16.3082427557362));
#21092=CARTESIAN_POINT('Ctrl Pts',(16.,-60.,-15.6204993518134));
#21093=CARTESIAN_POINT('Origin',(0.,-59.9290405600022,-17.4897180799923));
#21094=CARTESIAN_POINT('',(17.2600442058128,-59.858081116524,-17.9794361715722));
#21095=CARTESIAN_POINT('',(0.,-59.8580811200045,-17.9794361599846));
#21096=CARTESIAN_POINT('',(18.,-60.,-17.));
#21097=CARTESIAN_POINT('Origin',(18.,-58.,-30.8027605631545));
#21098=CARTESIAN_POINT('',(0.,-60.,-17.));
#21099=CARTESIAN_POINT('Origin',(16.,-60.,32.));
#21100=CARTESIAN_POINT('',(18.,-60.,-32.));
#21101=CARTESIAN_POINT('',(18.,-60.,16.));
#21102=CARTESIAN_POINT('',(123.8,-60.,-32.));
#21103=CARTESIAN_POINT('',(16.,-60.,-32.));
#21104=CARTESIAN_POINT('',(123.8,-60.,32.));
#21105=CARTESIAN_POINT('',(123.8,-60.,16.));
#21106=CARTESIAN_POINT('',(18.,-60.,32.));
#21107=CARTESIAN_POINT('',(16.,-60.,32.));
#21108=CARTESIAN_POINT('',(18.,-60.,17.));
#21109=CARTESIAN_POINT('',(18.,-60.,16.));
#21110=CARTESIAN_POINT('',(15.6381526893245,-60.,17.));
#21111=CARTESIAN_POINT('',(0.,-60.,17.));
#21112=CARTESIAN_POINT('Ctrl Pts',(16.,-60.,15.6204993518133));
#21113=CARTESIAN_POINT('Ctrl Pts',(15.826727493626,-60.,16.3082427557361));
#21114=CARTESIAN_POINT('Ctrl Pts',(15.6381526893245,-60.,17.));
#21115=CARTESIAN_POINT('Origin',(0.,-17.4897180799923,-59.9290405600022));
#21116=CARTESIAN_POINT('',(14.,-17.9794361599846,-59.8580811200045));
#21117=CARTESIAN_POINT('',(14.7304276784111,-16.9999999991831,-60.));
#21118=CARTESIAN_POINT('Ctrl Pts',(14.7304276776349,-16.9999999989424,-60.0000000001532));
#21119=CARTESIAN_POINT('Ctrl Pts',(14.6761902161882,-17.159755202079,-59.9768517027666));
#21120=CARTESIAN_POINT('Ctrl Pts',(14.6152171518727,-17.3169819821409,-59.9540697702187));
#21121=CARTESIAN_POINT('Ctrl Pts',(14.4632746479611,-17.6188900437764,-59.9103237296707));
#21122=CARTESIAN_POINT('Ctrl Pts',(14.3588395089388,-17.7908531163461,-59.8854065296971));
#21123=CARTESIAN_POINT('Ctrl Pts',(14.1914653455901,-17.9195593830331,-59.8667571781999));
#21124=CARTESIAN_POINT('Ctrl Pts',(14.1471388512752,-17.9457470523029,-59.8629626228789));
#21125=CARTESIAN_POINT('Ctrl Pts',(14.074547869931,-17.9718483805388,-59.8591805782485));
#21126=CARTESIAN_POINT('Ctrl Pts',(14.0342136843971,-17.9794361599847,-59.8580811200045));
#21127=CARTESIAN_POINT('Ctrl Pts',(14.,-17.9794361599847,-59.8580811200045));
#21128=CARTESIAN_POINT('',(18.,-17.,-60.));
#21129=CARTESIAN_POINT('',(0.,-17.,-60.));
#21130=CARTESIAN_POINT('',(17.2600442058128,-17.9794361715722,-59.858081116524));
#21131=CARTESIAN_POINT('Origin',(18.,-30.8027605631545,-58.));
#21132=CARTESIAN_POINT('',(0.,-17.9794361599846,-59.8580811200045));
#21133=CARTESIAN_POINT('Origin',(16.,-32.,-60.));
#21134=CARTESIAN_POINT('',(18.,-32.,-60.));
#21135=CARTESIAN_POINT('',(18.,-16.,-60.));
#21136=CARTESIAN_POINT('',(16.,-7.76208734813001,-60.));
#21137=CARTESIAN_POINT('Ctrl Pts',(14.7304276780283,-16.9999999989171,-60.));
#21138=CARTESIAN_POINT('Ctrl Pts',(14.8398686953361,-16.8424989931707,-60.));
#21139=CARTESIAN_POINT('Ctrl Pts',(14.9313718498422,-16.6679371205732,-60.));
#21140=CARTESIAN_POINT('Ctrl Pts',(15.2970561697214,-15.8666064940819,-60.));
#21141=CARTESIAN_POINT('Ctrl Pts',(15.4592365878721,-15.1702769231182,-60.));
#21142=CARTESIAN_POINT('Ctrl Pts',(15.7175697501628,-13.7281199101031,-60.));
#21143=CARTESIAN_POINT('Ctrl Pts',(15.8016080012342,-12.9801486404093,-60.));
#21144=CARTESIAN_POINT('Ctrl Pts',(15.9799340791093,-10.7101781630257,-60.));
#21145=CARTESIAN_POINT('Ctrl Pts',(16.,-9.16876356419723,-60.));
#21146=CARTESIAN_POINT('Ctrl Pts',(16.,-7.76208734813001,-60.));
#21147=CARTESIAN_POINT('',(16.,7.76208734813001,-60.));
#21148=CARTESIAN_POINT('',(16.,-16.,-60.));
#21149=CARTESIAN_POINT('',(14.7304276784111,16.9999999991831,-60.));
#21150=CARTESIAN_POINT('Ctrl Pts',(16.,7.76208734813,-60.));
#21151=CARTESIAN_POINT('Ctrl Pts',(16.,9.16876356419723,-60.));
#21152=CARTESIAN_POINT('Ctrl Pts',(15.9799340791093,10.7101781630257,-60.));
#21153=CARTESIAN_POINT('Ctrl Pts',(15.8016080012342,12.9801486404093,-60.));
#21154=CARTESIAN_POINT('Ctrl Pts',(15.7175697501628,13.7281199101031,-60.));
#21155=CARTESIAN_POINT('Ctrl Pts',(15.4592365878721,15.1702769231182,-60.));
#21156=CARTESIAN_POINT('Ctrl Pts',(15.2970561697214,15.8666064940819,-60.));
#21157=CARTESIAN_POINT('Ctrl Pts',(14.9313718498422,16.6679371205732,-60.));
#21158=CARTESIAN_POINT('Ctrl Pts',(14.8398686953361,16.8424989931707,-60.));
#21159=CARTESIAN_POINT('Ctrl Pts',(14.7304276780283,16.9999999989171,-60.));
#21160=CARTESIAN_POINT('',(18.,17.,-60.));
#21161=CARTESIAN_POINT('',(0.,17.,-60.));
#21162=CARTESIAN_POINT('',(18.,32.,-60.));
#21163=CARTESIAN_POINT('',(18.,-16.,-60.));
#21164=CARTESIAN_POINT('',(16.,32.,-60.));
#21165=CARTESIAN_POINT('',(123.8,32.,-60.));
#21166=CARTESIAN_POINT('',(16.,32.,-60.));
#21167=CARTESIAN_POINT('',(123.8,-32.,-60.));
#21168=CARTESIAN_POINT('',(123.8,-16.,-60.));
#21169=CARTESIAN_POINT('',(16.,-32.,-60.));
#21170=CARTESIAN_POINT('Origin',(0.,17.4897180799923,-59.9290405600022));
#21171=CARTESIAN_POINT('',(17.2600442058128,17.9794361715722,-59.858081116524));
#21172=CARTESIAN_POINT('Origin',(18.,30.8027605631545,-58.));
#21173=CARTESIAN_POINT('',(14.,17.9794361599846,-59.8580811200045));
#21174=CARTESIAN_POINT('Ctrl Pts',(14.,17.9794361599847,-59.8580811200045));
#21175=CARTESIAN_POINT('Ctrl Pts',(14.0342136843971,17.9794361599847,-59.8580811200045));
#21176=CARTESIAN_POINT('Ctrl Pts',(14.074547869931,17.9718483805388,-59.8591805782485));
#21177=CARTESIAN_POINT('Ctrl Pts',(14.1471388512752,17.9457470523029,-59.8629626228789));
#21178=CARTESIAN_POINT('Ctrl Pts',(14.1914653455901,17.9195593830331,-59.8667571781999));
#21179=CARTESIAN_POINT('Ctrl Pts',(14.3588395089388,17.7908531163461,-59.8854065296971));
#21180=CARTESIAN_POINT('Ctrl Pts',(14.4632746479611,17.6188900437764,-59.9103237296707));
#21181=CARTESIAN_POINT('Ctrl Pts',(14.6152171518727,17.3169819821409,-59.9540697702187));
#21182=CARTESIAN_POINT('Ctrl Pts',(14.6761902161882,17.159755202079,-59.9768517027666));
#21183=CARTESIAN_POINT('Ctrl Pts',(14.7304276776349,16.9999999989424,-60.0000000001532));
#21184=CARTESIAN_POINT('',(0.,17.9794361599846,-59.8580811200045));
#21185=CARTESIAN_POINT('Origin',(15.75,0.,0.));
#21186=CARTESIAN_POINT('',(15.5,59.8580811200045,-17.9794361599846));
#21187=CARTESIAN_POINT('',(15.4999999969433,61.0634996055951,-13.3228756624643));
#21188=CARTESIAN_POINT('Origin',(15.5,0.,0.));
#21189=CARTESIAN_POINT('Ctrl Pts',(16.,60.8276253029822,-11.9999999999999));
#21190=CARTESIAN_POINT('Ctrl Pts',(16.,60.80493204889,-12.1150313964023));
#21191=CARTESIAN_POINT('Ctrl Pts',(15.9898935814354,60.7916707113854,-12.2327047392017));
#21192=CARTESIAN_POINT('Ctrl Pts',(15.9261070025809,60.7835362526876,-12.5931700844189));
#21193=CARTESIAN_POINT('Ctrl Pts',(15.8336779042045,60.8282401952317,-12.8299273372329));
#21194=CARTESIAN_POINT('Ctrl Pts',(15.6534629211121,60.9478909731446,-13.1321977587055));
#21195=CARTESIAN_POINT('Ctrl Pts',(15.5800859964154,61.0013423773347,-13.2320666717072));
#21196=CARTESIAN_POINT('Ctrl Pts',(15.4999999966277,61.0634996097249,-13.3228756593561));
#21197=CARTESIAN_POINT('',(15.6381526893245,60.,-17.));
#21198=CARTESIAN_POINT('Ctrl Pts',(16.,60.,-15.6204993518133));
#21199=CARTESIAN_POINT('Ctrl Pts',(15.826727493626,60.,-16.3082427557361));
#21200=CARTESIAN_POINT('Ctrl Pts',(15.6381526893245,60.,-17.));
#21201=CARTESIAN_POINT('Ctrl Pts',(15.6381526893245,60.,-17.));
#21202=CARTESIAN_POINT('Ctrl Pts',(15.5946215988532,59.9526427924876,-17.3268300981166));
#21203=CARTESIAN_POINT('Ctrl Pts',(15.5485606843564,59.9053376415118,-17.6533009342783));
#21204=CARTESIAN_POINT('Ctrl Pts',(15.5,59.8580811200045,-17.9794361599846));
#21205=CARTESIAN_POINT('Origin',(0.,59.9290405600022,-17.4897180799923));
#21206=CARTESIAN_POINT('',(18.,60.,-17.));
#21207=CARTESIAN_POINT('',(0.,60.,-17.));
#21208=CARTESIAN_POINT('',(17.2600442058128,59.858081116524,-17.9794361715722));
#21209=CARTESIAN_POINT('Origin',(18.,58.,-30.8027605631545));
#21210=CARTESIAN_POINT('',(0.,59.8580811200045,-17.9794361599846));
#21211=CARTESIAN_POINT('Origin',(0.,0.,0.));
#21212=CARTESIAN_POINT('',(14.,-60.9118215127409,-14.));
#21213=CARTESIAN_POINT('Ctrl Pts',(15.499999995189,-61.0634996059174,-13.3228756609874));
#21214=CARTESIAN_POINT('Ctrl Pts',(15.4701909647076,-61.056125041613,-13.3566759242301));
#21215=CARTESIAN_POINT('Ctrl Pts',(15.4394885037721,-61.0490034120379,-13.3891821198367));
#21216=CARTESIAN_POINT('Ctrl Pts',(15.2319678738428,-61.0037715519876,-13.5949189134652));
#21217=CARTESIAN_POINT('Ctrl Pts',(15.008663619483,-60.9694430253741,-13.7472835331182));
#21218=CARTESIAN_POINT('Ctrl Pts',(14.5181770858478,-60.9234160168088,-13.9498447390067));
#21219=CARTESIAN_POINT('Ctrl Pts',(14.2509679895827,-60.9118215127409,-14.));
#21220=CARTESIAN_POINT('Ctrl Pts',(14.,-60.9118215127409,-14.));
#21221=CARTESIAN_POINT('',(2.,-60.9118215127409,-14.));
#21222=CARTESIAN_POINT('',(0.,-60.9118215127409,-14.));
#21223=CARTESIAN_POINT('',(2.,60.9118215127409,-14.));
#21224=CARTESIAN_POINT('Origin',(2.,0.,0.));
#21225=CARTESIAN_POINT('',(14.,60.9118215127409,-14.));
#21226=CARTESIAN_POINT('',(0.,60.9118215127409,-14.));
#21227=CARTESIAN_POINT('Ctrl Pts',(14.,60.9118215127409,-14.));
#21228=CARTESIAN_POINT('Ctrl Pts',(14.2509679895827,60.9118215127409,-14.));
#21229=CARTESIAN_POINT('Ctrl Pts',(14.5181770858478,60.9234160168088,-13.9498447390067));
#21230=CARTESIAN_POINT('Ctrl Pts',(15.008663619483,60.9694430253741,-13.7472835331182));
#21231=CARTESIAN_POINT('Ctrl Pts',(15.2319678738428,61.0037715519876,-13.5949189134652));
#21232=CARTESIAN_POINT('Ctrl Pts',(15.4394885037721,61.0490034120379,-13.3891821198367));
#21233=CARTESIAN_POINT('Ctrl Pts',(15.4701909647076,61.056125041613,-13.3566759242301));
#21234=CARTESIAN_POINT('Ctrl Pts',(15.499999995189,61.0634996059174,-13.3228756609874));
#21235=CARTESIAN_POINT('',(16.,58.,-23.28626204439));
#21236=CARTESIAN_POINT('Ctrl Pts',(17.2600442115558,59.8580811153305,-17.9794361755454));
#21237=CARTESIAN_POINT('Ctrl Pts',(17.127243690827,59.8051950958716,-18.1555070829828));
#21238=CARTESIAN_POINT('Ctrl Pts',(17.0139600323404,59.7441024880535,-18.3559136759436));
#21239=CARTESIAN_POINT('Ctrl Pts',(16.7810925644696,59.5935235342901,-18.8400023150408));
#21240=CARTESIAN_POINT('Ctrl Pts',(16.6727999393301,59.5012270640763,-19.1293647114412));
#21241=CARTESIAN_POINT('Ctrl Pts',(16.195648993787,59.0240761185332,-20.5909899649672));
#21242=CARTESIAN_POINT('Ctrl Pts',(16.,58.4904260224498,-22.0647388455243));
#21243=CARTESIAN_POINT('Ctrl Pts',(16.,58.,-23.28626204439));
#21244=CARTESIAN_POINT('',(16.,23.28626204439,-58.));
#21245=CARTESIAN_POINT('Origin',(16.,0.,0.));
#21246=CARTESIAN_POINT('Ctrl Pts',(16.,23.28626204439,-58.));
#21247=CARTESIAN_POINT('Ctrl Pts',(16.,22.0647388455243,-58.4904260224498));
#21248=CARTESIAN_POINT('Ctrl Pts',(16.195648993787,20.5909899649672,-59.0240761185332));
#21249=CARTESIAN_POINT('Ctrl Pts',(16.6727999393301,19.1293647114412,-59.5012270640763));
#21250=CARTESIAN_POINT('Ctrl Pts',(16.7810925644696,18.8400023150408,-59.5935235342901));
#21251=CARTESIAN_POINT('Ctrl Pts',(17.0139600323404,18.3559136759436,-59.7441024880535));
#21252=CARTESIAN_POINT('Ctrl Pts',(17.127243690827,18.1555070829828,-59.8051950958716));
#21253=CARTESIAN_POINT('Ctrl Pts',(17.2600442115558,17.9794361755454,-59.8580811153305));
#21254=CARTESIAN_POINT('Origin',(14.,0.,0.));
#21255=CARTESIAN_POINT('',(16.,-23.28626204439,-58.));
#21256=CARTESIAN_POINT('Ctrl Pts',(17.2600442115558,-17.9794361755454,-59.8580811153305));
#21257=CARTESIAN_POINT('Ctrl Pts',(17.127243690827,-18.1555070829828,-59.8051950958716));
#21258=CARTESIAN_POINT('Ctrl Pts',(17.0139600323404,-18.3559136759436,-59.7441024880535));
#21259=CARTESIAN_POINT('Ctrl Pts',(16.7810925644696,-18.8400023150408,-59.5935235342901));
#21260=CARTESIAN_POINT('Ctrl Pts',(16.6727999393301,-19.1293647114412,-59.5012270640763));
#21261=CARTESIAN_POINT('Ctrl Pts',(16.195648993787,-20.5909899649672,-59.0240761185332));
#21262=CARTESIAN_POINT('Ctrl Pts',(16.,-22.0647388455243,-58.4904260224498));
#21263=CARTESIAN_POINT('Ctrl Pts',(16.,-23.28626204439,-58.));
#21264=CARTESIAN_POINT('',(16.,-58.,-23.28626204439));
#21265=CARTESIAN_POINT('Origin',(16.,0.,0.));
#21266=CARTESIAN_POINT('Ctrl Pts',(16.,-58.,-23.28626204439));
#21267=CARTESIAN_POINT('Ctrl Pts',(16.,-58.4904260224498,-22.0647388455243));
#21268=CARTESIAN_POINT('Ctrl Pts',(16.195648993787,-59.0240761185332,-20.5909899649672));
#21269=CARTESIAN_POINT('Ctrl Pts',(16.6727999393301,-59.5012270640763,-19.1293647114412));
#21270=CARTESIAN_POINT('Ctrl Pts',(16.7810925644696,-59.5935235342901,-18.8400023150408));
#21271=CARTESIAN_POINT('Ctrl Pts',(17.0139600323404,-59.7441024880535,-18.3559136759436));
#21272=CARTESIAN_POINT('Ctrl Pts',(17.127243690827,-59.8051950958716,-18.1555070829828));
#21273=CARTESIAN_POINT('Ctrl Pts',(17.2600442115558,-59.8580811153305,-17.9794361755454));
#21274=CARTESIAN_POINT('Origin',(15.75,0.,0.));
#21275=CARTESIAN_POINT('',(15.4999999969433,61.0634996055951,13.3228756624643));
#21276=CARTESIAN_POINT('Ctrl Pts',(15.4999999966277,61.0634996097249,13.3228756593561));
#21277=CARTESIAN_POINT('Ctrl Pts',(15.5800859964154,61.0013423773347,13.2320666717072));
#21278=CARTESIAN_POINT('Ctrl Pts',(15.6534629211121,60.9478909731446,13.1321977587055));
#21279=CARTESIAN_POINT('Ctrl Pts',(15.8336779042045,60.8282401952317,12.8299273372328));
#21280=CARTESIAN_POINT('Ctrl Pts',(15.9261070025809,60.7835362526876,12.5931700844189));
#21281=CARTESIAN_POINT('Ctrl Pts',(15.9898935814354,60.7916707113854,12.2327047392017));
#21282=CARTESIAN_POINT('Ctrl Pts',(16.,60.80493204889,12.1150313964023));
#21283=CARTESIAN_POINT('Ctrl Pts',(16.,60.8276253029822,11.9999999999999));
#21284=CARTESIAN_POINT('',(15.5,59.8580811200045,17.9794361599846));
#21285=CARTESIAN_POINT('Origin',(15.5,0.,0.));
#21286=CARTESIAN_POINT('',(15.6381526893245,60.,17.));
#21287=CARTESIAN_POINT('Ctrl Pts',(15.5,59.8580811200045,17.9794361599846));
#21288=CARTESIAN_POINT('Ctrl Pts',(15.5485606843564,59.9053376415117,17.6533009342786));
#21289=CARTESIAN_POINT('Ctrl Pts',(15.5946215988532,59.9526427924876,17.3268300981168));
#21290=CARTESIAN_POINT('Ctrl Pts',(15.6381526893245,60.,17.));
#21291=CARTESIAN_POINT('Ctrl Pts',(15.6381526893245,60.,17.));
#21292=CARTESIAN_POINT('Ctrl Pts',(15.826727493626,60.,16.3082427557361));
#21293=CARTESIAN_POINT('Ctrl Pts',(16.,60.,15.6204993518132));
#21294=CARTESIAN_POINT('Origin',(0.,59.9290405600022,17.4897180799923));
#21295=CARTESIAN_POINT('',(17.2600442058128,59.858081116524,17.9794361715722));
#21296=CARTESIAN_POINT('',(0.,59.8580811200045,17.9794361599846));
#21297=CARTESIAN_POINT('',(18.,60.,17.));
#21298=CARTESIAN_POINT('Origin',(18.,58.,30.8027605631545));
#21299=CARTESIAN_POINT('',(0.,60.,17.));
#21300=CARTESIAN_POINT('Origin',(16.,60.,-32.));
#21301=CARTESIAN_POINT('',(18.,60.,32.));
#21302=CARTESIAN_POINT('',(18.,60.,-16.));
#21303=CARTESIAN_POINT('',(123.8,60.,32.));
#21304=CARTESIAN_POINT('',(16.,60.,32.));
#21305=CARTESIAN_POINT('',(123.8,60.,-32.));
#21306=CARTESIAN_POINT('',(123.8,60.,-16.));
#21307=CARTESIAN_POINT('',(18.,60.,-32.));
#21308=CARTESIAN_POINT('',(16.,60.,-32.));
#21309=CARTESIAN_POINT('',(18.,60.,-16.));
#21310=CARTESIAN_POINT('Origin',(0.,17.4897180799923,59.9290405600022));
#21311=CARTESIAN_POINT('',(14.,17.9794361599846,59.8580811200045));
#21312=CARTESIAN_POINT('',(14.7304276784111,16.9999999991831,60.));
#21313=CARTESIAN_POINT('Ctrl Pts',(14.7304276776349,16.9999999989424,60.0000000001532));
#21314=CARTESIAN_POINT('Ctrl Pts',(14.6761902161882,17.159755202079,59.9768517027666));
#21315=CARTESIAN_POINT('Ctrl Pts',(14.6152171518727,17.3169819821409,59.9540697702187));
#21316=CARTESIAN_POINT('Ctrl Pts',(14.4632746479611,17.6188900437764,59.9103237296707));
#21317=CARTESIAN_POINT('Ctrl Pts',(14.3588395089388,17.7908531163461,59.8854065296971));
#21318=CARTESIAN_POINT('Ctrl Pts',(14.1914653455901,17.9195593830331,59.8667571781999));
#21319=CARTESIAN_POINT('Ctrl Pts',(14.1471388512752,17.9457470523029,59.8629626228789));
#21320=CARTESIAN_POINT('Ctrl Pts',(14.074547869931,17.9718483805388,59.8591805782485));
#21321=CARTESIAN_POINT('Ctrl Pts',(14.0342136843971,17.9794361599847,59.8580811200045));
#21322=CARTESIAN_POINT('Ctrl Pts',(14.,17.9794361599847,59.8580811200045));
#21323=CARTESIAN_POINT('',(18.,17.,60.));
#21324=CARTESIAN_POINT('',(0.,17.,60.));
#21325=CARTESIAN_POINT('',(17.2600442058128,17.9794361715722,59.858081116524));
#21326=CARTESIAN_POINT('Origin',(18.,30.8027605631545,58.));
#21327=CARTESIAN_POINT('',(0.,17.9794361599846,59.8580811200045));
#21328=CARTESIAN_POINT('Origin',(16.,32.,60.));
#21329=CARTESIAN_POINT('',(18.,32.,60.));
#21330=CARTESIAN_POINT('',(18.,16.,60.));
#21331=CARTESIAN_POINT('',(16.,7.76208734813001,60.));
#21332=CARTESIAN_POINT('Ctrl Pts',(14.7304276780283,16.9999999989171,60.));
#21333=CARTESIAN_POINT('Ctrl Pts',(14.8398686953361,16.8424989931707,60.));
#21334=CARTESIAN_POINT('Ctrl Pts',(14.9313718498422,16.6679371205732,60.));
#21335=CARTESIAN_POINT('Ctrl Pts',(15.2970561697214,15.8666064940819,60.));
#21336=CARTESIAN_POINT('Ctrl Pts',(15.4592365878721,15.1702769231182,60.));
#21337=CARTESIAN_POINT('Ctrl Pts',(15.7175697501628,13.7281199101031,60.));
#21338=CARTESIAN_POINT('Ctrl Pts',(15.8016080012342,12.9801486404093,60.));
#21339=CARTESIAN_POINT('Ctrl Pts',(15.9799340791093,10.7101781630257,60.));
#21340=CARTESIAN_POINT('Ctrl Pts',(16.,9.16876356419723,60.));
#21341=CARTESIAN_POINT('Ctrl Pts',(16.,7.76208734813001,60.));
#21342=CARTESIAN_POINT('',(16.,-7.76208734813001,60.));
#21343=CARTESIAN_POINT('',(16.,16.,60.));
#21344=CARTESIAN_POINT('',(14.7304276784111,-16.9999999991831,60.));
#21345=CARTESIAN_POINT('Ctrl Pts',(16.,-7.76208734813,60.));
#21346=CARTESIAN_POINT('Ctrl Pts',(16.,-9.16876356419723,60.));
#21347=CARTESIAN_POINT('Ctrl Pts',(15.9799340791093,-10.7101781630257,60.));
#21348=CARTESIAN_POINT('Ctrl Pts',(15.8016080012342,-12.9801486404093,60.));
#21349=CARTESIAN_POINT('Ctrl Pts',(15.7175697501628,-13.7281199101031,60.));
#21350=CARTESIAN_POINT('Ctrl Pts',(15.4592365878721,-15.1702769231182,60.));
#21351=CARTESIAN_POINT('Ctrl Pts',(15.2970561697214,-15.8666064940819,60.));
#21352=CARTESIAN_POINT('Ctrl Pts',(14.9313718498422,-16.6679371205732,60.));
#21353=CARTESIAN_POINT('Ctrl Pts',(14.8398686953361,-16.8424989931707,60.));
#21354=CARTESIAN_POINT('Ctrl Pts',(14.7304276780283,-16.9999999989171,60.));
#21355=CARTESIAN_POINT('',(18.,-17.,60.));
#21356=CARTESIAN_POINT('',(0.,-17.,60.));
#21357=CARTESIAN_POINT('',(18.,-32.,60.));
#21358=CARTESIAN_POINT('',(18.,16.,60.));
#21359=CARTESIAN_POINT('',(123.8,-32.,60.));
#21360=CARTESIAN_POINT('',(16.,-32.,60.));
#21361=CARTESIAN_POINT('',(123.8,32.,60.));
#21362=CARTESIAN_POINT('',(123.8,16.,60.));
#21363=CARTESIAN_POINT('',(16.,32.,60.));
#21364=CARTESIAN_POINT('',(16.,32.,60.));
#21365=CARTESIAN_POINT('Origin',(0.,-17.4897180799923,59.9290405600022));
#21366=CARTESIAN_POINT('',(17.2600442058128,-17.9794361715722,59.858081116524));
#21367=CARTESIAN_POINT('Origin',(18.,-30.8027605631545,58.));
#21368=CARTESIAN_POINT('',(14.,-17.9794361599846,59.8580811200045));
#21369=CARTESIAN_POINT('Ctrl Pts',(14.,-17.9794361599847,59.8580811200045));
#21370=CARTESIAN_POINT('Ctrl Pts',(14.0342136843971,-17.9794361599847,59.8580811200045));
#21371=CARTESIAN_POINT('Ctrl Pts',(14.074547869931,-17.9718483805388,59.8591805782485));
#21372=CARTESIAN_POINT('Ctrl Pts',(14.1471388512752,-17.9457470523029,59.8629626228789));
#21373=CARTESIAN_POINT('Ctrl Pts',(14.1914653455901,-17.9195593830331,59.8667571781999));
#21374=CARTESIAN_POINT('Ctrl Pts',(14.3588395089388,-17.7908531163461,59.8854065296971));
#21375=CARTESIAN_POINT('Ctrl Pts',(14.4632746479611,-17.6188900437764,59.9103237296707));
#21376=CARTESIAN_POINT('Ctrl Pts',(14.6152171518727,-17.3169819821409,59.9540697702187));
#21377=CARTESIAN_POINT('Ctrl Pts',(14.6761902161882,-17.159755202079,59.9768517027666));
#21378=CARTESIAN_POINT('Ctrl Pts',(14.7304276776349,-16.9999999989424,60.0000000001532));
#21379=CARTESIAN_POINT('',(0.,-17.9794361599846,59.8580811200045));
#21380=CARTESIAN_POINT('Origin',(15.75,0.,0.));
#21381=CARTESIAN_POINT('',(15.5,-59.8580811200045,17.9794361599846));
#21382=CARTESIAN_POINT('',(15.4999999969433,-61.0634996055951,13.3228756624643));
#21383=CARTESIAN_POINT('Origin',(15.5,0.,0.));
#21384=CARTESIAN_POINT('Ctrl Pts',(16.,-60.8276253029822,11.9999999999999));
#21385=CARTESIAN_POINT('Ctrl Pts',(16.,-60.8049320488899,12.1150313964023));
#21386=CARTESIAN_POINT('Ctrl Pts',(15.9898935814354,-60.7916707113854,12.2327047392017));
#21387=CARTESIAN_POINT('Ctrl Pts',(15.9261070025809,-60.7835362526876,12.5931700844189));
#21388=CARTESIAN_POINT('Ctrl Pts',(15.8336779042045,-60.8282401952317,12.8299273372328));
#21389=CARTESIAN_POINT('Ctrl Pts',(15.6534629211121,-60.9478909731446,13.1321977587055));
#21390=CARTESIAN_POINT('Ctrl Pts',(15.5800859964154,-61.0013423773347,13.2320666717072));
#21391=CARTESIAN_POINT('Ctrl Pts',(15.4999999966277,-61.0634996097249,13.3228756593561));
#21392=CARTESIAN_POINT('Ctrl Pts',(15.6381526893245,-60.,17.));
#21393=CARTESIAN_POINT('Ctrl Pts',(15.5946215988532,-59.9526427924876,17.3268300981168));
#21394=CARTESIAN_POINT('Ctrl Pts',(15.5485606843564,-59.9053376415117,17.6533009342786));
#21395=CARTESIAN_POINT('Ctrl Pts',(15.5,-59.8580811200045,17.9794361599846));
#21396=CARTESIAN_POINT('Origin',(0.,-59.9290405600022,17.4897180799923));
#21397=CARTESIAN_POINT('',(17.2600442058128,-59.858081116524,17.9794361715722));
#21398=CARTESIAN_POINT('Origin',(18.,-58.,30.8027605631545));
#21399=CARTESIAN_POINT('',(0.,-59.8580811200045,17.9794361599846));
#21400=CARTESIAN_POINT('Origin',(0.,0.,0.));
#21401=CARTESIAN_POINT('',(14.,60.9118215127409,14.));
#21402=CARTESIAN_POINT('Ctrl Pts',(15.499999995189,61.0634996059174,13.3228756609874));
#21403=CARTESIAN_POINT('Ctrl Pts',(15.4701909647076,61.056125041613,13.3566759242301));
#21404=CARTESIAN_POINT('Ctrl Pts',(15.4394885037721,61.0490034120379,13.3891821198367));
#21405=CARTESIAN_POINT('Ctrl Pts',(15.2319678738428,61.0037715519876,13.5949189134652));
#21406=CARTESIAN_POINT('Ctrl Pts',(15.008663619483,60.9694430253741,13.7472835331182));
#21407=CARTESIAN_POINT('Ctrl Pts',(14.5181770858478,60.9234160168088,13.9498447390067));
#21408=CARTESIAN_POINT('Ctrl Pts',(14.2509679895827,60.9118215127409,14.));
#21409=CARTESIAN_POINT('Ctrl Pts',(14.,60.9118215127409,14.));
#21410=CARTESIAN_POINT('',(2.,60.9118215127409,14.));
#21411=CARTESIAN_POINT('',(0.,60.9118215127409,14.));
#21412=CARTESIAN_POINT('',(2.,-60.9118215127409,14.));
#21413=CARTESIAN_POINT('Origin',(2.,0.,0.));
#21414=CARTESIAN_POINT('',(14.,-60.9118215127409,14.));
#21415=CARTESIAN_POINT('',(0.,-60.9118215127409,14.));
#21416=CARTESIAN_POINT('Ctrl Pts',(14.,-60.9118215127409,14.));
#21417=CARTESIAN_POINT('Ctrl Pts',(14.2509679895827,-60.9118215127409,14.));
#21418=CARTESIAN_POINT('Ctrl Pts',(14.5181770858478,-60.9234160168088,13.9498447390067));
#21419=CARTESIAN_POINT('Ctrl Pts',(15.008663619483,-60.9694430253741,13.7472835331182));
#21420=CARTESIAN_POINT('Ctrl Pts',(15.2319678738428,-61.0037715519876,13.5949189134652));
#21421=CARTESIAN_POINT('Ctrl Pts',(15.4394885037721,-61.0490034120379,13.3891821198367));
#21422=CARTESIAN_POINT('Ctrl Pts',(15.4701909647076,-61.056125041613,13.3566759242301));
#21423=CARTESIAN_POINT('Ctrl Pts',(15.499999995189,-61.0634996059174,13.3228756609874));
#21424=CARTESIAN_POINT('',(16.,-58.,23.28626204439));
#21425=CARTESIAN_POINT('Ctrl Pts',(17.2600442115558,-59.8580811153305,17.9794361755454));
#21426=CARTESIAN_POINT('Ctrl Pts',(17.127243690827,-59.8051950958716,18.1555070829828));
#21427=CARTESIAN_POINT('Ctrl Pts',(17.0139600323404,-59.7441024880535,18.3559136759436));
#21428=CARTESIAN_POINT('Ctrl Pts',(16.7810925644696,-59.5935235342901,18.8400023150408));
#21429=CARTESIAN_POINT('Ctrl Pts',(16.6727999393301,-59.5012270640763,19.1293647114412));
#21430=CARTESIAN_POINT('Ctrl Pts',(16.195648993787,-59.0240761185332,20.5909899649672));
#21431=CARTESIAN_POINT('Ctrl Pts',(16.,-58.4904260224498,22.0647388455243));
#21432=CARTESIAN_POINT('Ctrl Pts',(16.,-58.,23.28626204439));
#21433=CARTESIAN_POINT('',(16.,-23.28626204439,58.));
#21434=CARTESIAN_POINT('Origin',(16.,0.,0.));
#21435=CARTESIAN_POINT('Ctrl Pts',(16.,-23.28626204439,58.));
#21436=CARTESIAN_POINT('Ctrl Pts',(16.,-22.0647388455243,58.4904260224498));
#21437=CARTESIAN_POINT('Ctrl Pts',(16.195648993787,-20.5909899649672,59.0240761185332));
#21438=CARTESIAN_POINT('Ctrl Pts',(16.6727999393301,-19.1293647114412,59.5012270640763));
#21439=CARTESIAN_POINT('Ctrl Pts',(16.7810925644696,-18.8400023150408,59.5935235342901));
#21440=CARTESIAN_POINT('Ctrl Pts',(17.0139600323404,-18.3559136759436,59.7441024880535));
#21441=CARTESIAN_POINT('Ctrl Pts',(17.127243690827,-18.1555070829828,59.8051950958716));
#21442=CARTESIAN_POINT('Ctrl Pts',(17.2600442115558,-17.9794361755454,59.8580811153305));
#21443=CARTESIAN_POINT('Origin',(14.,0.,0.));
#21444=CARTESIAN_POINT('',(16.,23.28626204439,58.));
#21445=CARTESIAN_POINT('Ctrl Pts',(17.2600442115558,17.9794361755454,59.8580811153305));
#21446=CARTESIAN_POINT('Ctrl Pts',(17.127243690827,18.1555070829828,59.8051950958716));
#21447=CARTESIAN_POINT('Ctrl Pts',(17.0139600323404,18.3559136759436,59.7441024880535));
#21448=CARTESIAN_POINT('Ctrl Pts',(16.7810925644696,18.8400023150408,59.5935235342901));
#21449=CARTESIAN_POINT('Ctrl Pts',(16.6727999393301,19.1293647114412,59.5012270640763));
#21450=CARTESIAN_POINT('Ctrl Pts',(16.195648993787,20.5909899649672,59.0240761185332));
#21451=CARTESIAN_POINT('Ctrl Pts',(16.,22.0647388455243,58.4904260224498));
#21452=CARTESIAN_POINT('Ctrl Pts',(16.,23.28626204439,58.));
#21453=CARTESIAN_POINT('',(16.,58.,23.28626204439));
#21454=CARTESIAN_POINT('Origin',(16.,0.,0.));
#21455=CARTESIAN_POINT('Ctrl Pts',(16.,58.,23.28626204439));
#21456=CARTESIAN_POINT('Ctrl Pts',(16.,58.4904260224498,22.0647388455243));
#21457=CARTESIAN_POINT('Ctrl Pts',(16.195648993787,59.0240761185332,20.5909899649672));
#21458=CARTESIAN_POINT('Ctrl Pts',(16.6727999393301,59.5012270640763,19.1293647114412));
#21459=CARTESIAN_POINT('Ctrl Pts',(16.7810925644696,59.5935235342901,18.8400023150408));
#21460=CARTESIAN_POINT('Ctrl Pts',(17.0139600323404,59.7441024880535,18.3559136759436));
#21461=CARTESIAN_POINT('Ctrl Pts',(17.127243690827,59.8051950958716,18.1555070829828));
#21462=CARTESIAN_POINT('Ctrl Pts',(17.2600442115558,59.8580811153305,17.9794361755454));
#21463=CARTESIAN_POINT('Origin',(0.25,73.,0.));
#21464=CARTESIAN_POINT('',(0.,73.,7.65));
#21465=CARTESIAN_POINT('Origin',(0.,73.,0.));
#21466=CARTESIAN_POINT('',(0.25,73.,7.4));
#21467=CARTESIAN_POINT('Origin',(0.,0.,0.));
#21468=CARTESIAN_POINT('',(0.,-59.2979763567021,-12.));
#21469=CARTESIAN_POINT('',(0.,59.2979763567021,-12.));
#21470=CARTESIAN_POINT('Origin',(0.,0.,0.));
#21471=CARTESIAN_POINT('',(0.,-73.,-12.));
#21472=CARTESIAN_POINT('',(0.,-36.5,-12.));
#21473=CARTESIAN_POINT('',(0.,-73.,12.));
#21474=CARTESIAN_POINT('Origin',(0.,-73.,0.));
#21475=CARTESIAN_POINT('',(0.,-59.2979763567021,12.));
#21476=CARTESIAN_POINT('',(0.,-30.4559107563704,12.));
#21477=CARTESIAN_POINT('',(0.,59.2979763567021,12.));
#21478=CARTESIAN_POINT('Origin',(0.,0.,0.));
#21479=CARTESIAN_POINT('',(0.,73.,12.));
#21480=CARTESIAN_POINT('',(0.,36.5,12.));
#21481=CARTESIAN_POINT('',(0.,73.,-12.));
#21482=CARTESIAN_POINT('Origin',(0.,73.,0.));
#21483=CARTESIAN_POINT('',(0.,30.4559107563704,-12.));
#21484=CARTESIAN_POINT('',(0.,-73.,7.65));
#21485=CARTESIAN_POINT('Origin',(0.,-73.,0.));
#21486=CARTESIAN_POINT('',(0.,-50.8,-6.22120573966855E-15));
#21487=CARTESIAN_POINT('Origin',(0.,0.,0.));
#21488=CARTESIAN_POINT('Origin',(0.25,-73.,0.));
#21489=CARTESIAN_POINT('',(0.25,-73.,7.4));
#21490=CARTESIAN_POINT('Origin',(2.,0.,0.));
#21491=CARTESIAN_POINT('Ctrl Pts',(0.,59.2979763567021,12.));
#21492=CARTESIAN_POINT('Ctrl Pts',(1.25769149714818E-19,59.2996563019776,
12.0020539660872));
#21493=CARTESIAN_POINT('Ctrl Pts',(3.16408251292899E-6,59.3013362050753,
12.0041079678913));
#21494=CARTESIAN_POINT('Ctrl Pts',(0.000593503086363685,59.4580375808494,
12.1957134154004));
#21495=CARTESIAN_POINT('Ctrl Pts',(0.0281275031880837,59.613099217075,12.3860723403774));
#21496=CARTESIAN_POINT('Ctrl Pts',(0.136930554908868,59.909363508568,12.7511394004012));
#21497=CARTESIAN_POINT('Ctrl Pts',(0.216940282823655,60.0515916827231,12.9270721110806));
#21498=CARTESIAN_POINT('Ctrl Pts',(0.453050831357439,60.3435366239898,13.289351801108));
#21499=CARTESIAN_POINT('Ctrl Pts',(0.62144513700417,60.489695948914,13.4715348257732));
#21500=CARTESIAN_POINT('Ctrl Pts',(0.997206971331434,60.7067257339414,13.7427542799031));
#21501=CARTESIAN_POINT('Ctrl Pts',(1.1889063272169,60.7855458921753,13.8415441416268));
#21502=CARTESIAN_POINT('Ctrl Pts',(1.59182238859041,60.8864806167547,13.9681569376795));
#21503=CARTESIAN_POINT('Ctrl Pts',(1.79387301431878,60.9118215127408,14.));
#21504=CARTESIAN_POINT('Ctrl Pts',(2.,60.9118215127408,14.));
#21505=CARTESIAN_POINT('Ctrl Pts',(0.,-59.2979763567021,12.));
#21506=CARTESIAN_POINT('Ctrl Pts',(1.29042483160331E-19,-59.299700025109,
12.0021074236792));
#21507=CARTESIAN_POINT('Ctrl Pts',(3.33092592262858E-6,-59.3014236491314,
12.0042148849801));
#21508=CARTESIAN_POINT('Ctrl Pts',(0.000607509495687525,-59.4577300699319,
12.1953378269261));
#21509=CARTESIAN_POINT('Ctrl Pts',(0.0280029022425828,-59.6123506019909,
12.3851534403357));
#21510=CARTESIAN_POINT('Ctrl Pts',(0.135984528957224,-59.9071803866406,
12.7484458568845));
#21511=CARTESIAN_POINT('Ctrl Pts',(0.215085926484061,-60.0484388333809,
12.9231705561954));
#21512=CARTESIAN_POINT('Ctrl Pts',(0.449932961616034,-60.3406955295315,
13.2858134156949));
#21513=CARTESIAN_POINT('Ctrl Pts',(0.618802310815173,-60.4878960201855,
13.4692879696251));
#21514=CARTESIAN_POINT('Ctrl Pts',(0.995804745415966,-60.7061337709478,
13.7420125229231));
#21515=CARTESIAN_POINT('Ctrl Pts',(1.18797810444438,-60.7852814744256,13.8412125450258));
#21516=CARTESIAN_POINT('Ctrl Pts',(1.59159091693634,-60.8864513713538,13.9681201712759));
#21517=CARTESIAN_POINT('Ctrl Pts',(1.79375386609647,-60.9118215127408,14.));
#21518=CARTESIAN_POINT('Ctrl Pts',(2.,-60.9118215127408,14.));
#21519=CARTESIAN_POINT('Origin',(2.,-30.4559107563704,12.));
#21520=CARTESIAN_POINT('',(2.,-73.,14.));
#21521=CARTESIAN_POINT('Origin',(2.,-73.,12.));
#21522=CARTESIAN_POINT('',(2.,-30.4559107563704,14.));
#21523=CARTESIAN_POINT('Origin',(2.,-73.,0.));
#21524=CARTESIAN_POINT('',(2.,-73.,-14.));
#21525=CARTESIAN_POINT('Origin',(2.,-73.,-12.));
#21526=CARTESIAN_POINT('Origin',(2.,-73.,0.));
#21527=CARTESIAN_POINT('Origin',(2.,-36.5,-12.));
#21528=CARTESIAN_POINT('Ctrl Pts',(2.,-60.9118215127409,-14.));
#21529=CARTESIAN_POINT('Ctrl Pts',(1.79662005343113,-60.9118215127409,-14.));
#21530=CARTESIAN_POINT('Ctrl Pts',(1.59716111634269,-60.8871502501852,-13.9689987706081));
#21531=CARTESIAN_POINT('Ctrl Pts',(1.20761476381752,-60.7909127959859,-13.8482745236258));
#21532=CARTESIAN_POINT('Ctrl Pts',(1.02476537018483,-60.7182038738797,-13.7571370843373));
#21533=CARTESIAN_POINT('Ctrl Pts',(0.667985559569145,-60.5210049472671,
-13.5106227806572));
#21534=CARTESIAN_POINT('Ctrl Pts',(0.506200805332197,-60.3904050016375,
-13.347738482477));
#21535=CARTESIAN_POINT('Ctrl Pts',(0.249110343832778,-60.10362247768,-12.9914917064196));
#21536=CARTESIAN_POINT('Ctrl Pts',(0.154074961880266,-59.9469693395654,
-12.7975571845823));
#21537=CARTESIAN_POINT('Ctrl Pts',(0.0308705553692023,-59.6282594152053,
-12.4046866976145));
#21538=CARTESIAN_POINT('Ctrl Pts',(0.0006041682808588,-59.465531757485,
-12.2048763799246));
#21539=CARTESIAN_POINT('Ctrl Pts',(2.98520635993023E-6,-59.3012398529037,
-12.0039901590642));
#21540=CARTESIAN_POINT('Ctrl Pts',(-8.73769579204139E-18,-59.2996081247075,
-12.0019950626929));
#21541=CARTESIAN_POINT('Ctrl Pts',(0.,-59.2979763567021,-12.));
#21542=CARTESIAN_POINT('',(2.,-36.5,-14.));
#21543=CARTESIAN_POINT('Origin',(2.,0.,0.));
#21544=CARTESIAN_POINT('Ctrl Pts',(0.,59.2979763567021,-12.));
#21545=CARTESIAN_POINT('Ctrl Pts',(-9.22979868187932E-18,59.299700025109,
-12.0021074236792));
#21546=CARTESIAN_POINT('Ctrl Pts',(3.3309259227759E-6,59.3014236491314,
-12.0042148849801));
#21547=CARTESIAN_POINT('Ctrl Pts',(0.000607509495675756,59.4577300699289,
-12.1953378269221));
#21548=CARTESIAN_POINT('Ctrl Pts',(0.0280029022423892,59.6123506019904,
-12.385153440335));
#21549=CARTESIAN_POINT('Ctrl Pts',(0.135984528957217,59.9071803866406,-12.7484458568844));
#21550=CARTESIAN_POINT('Ctrl Pts',(0.215085926484053,60.0484388333809,-12.9231705561954));
#21551=CARTESIAN_POINT('Ctrl Pts',(0.449932961616014,60.3406955295314,-13.2858134156948));
#21552=CARTESIAN_POINT('Ctrl Pts',(0.618802310815157,60.4878960201855,-13.4692879696251));
#21553=CARTESIAN_POINT('Ctrl Pts',(0.995804745415989,60.7061337709478,-13.7420125229231));
#21554=CARTESIAN_POINT('Ctrl Pts',(1.18797810444439,60.7852814744256,-13.8412125450258));
#21555=CARTESIAN_POINT('Ctrl Pts',(1.59159091693627,60.8864513713538,-13.9681201712759));
#21556=CARTESIAN_POINT('Ctrl Pts',(1.79375386609643,60.9118215127409,-14.));
#21557=CARTESIAN_POINT('Ctrl Pts',(2.,60.9118215127409,-14.));
#21558=CARTESIAN_POINT('Origin',(2.,73.,0.));
#21559=CARTESIAN_POINT('',(2.,73.,-14.));
#21560=CARTESIAN_POINT('Origin',(2.,73.,-12.));
#21561=CARTESIAN_POINT('',(2.,73.,14.));
#21562=CARTESIAN_POINT('Origin',(2.,73.,12.));
#21563=CARTESIAN_POINT('Origin',(2.,73.,0.));
#21564=CARTESIAN_POINT('Origin',(2.,36.5,12.));
#21565=CARTESIAN_POINT('',(2.,36.5,14.));
#21566=CARTESIAN_POINT('Origin',(2.,30.4559107563704,-12.));
#21567=CARTESIAN_POINT('',(2.,30.4559107563704,-14.));
#21568=CARTESIAN_POINT('Origin',(0.,73.,0.));
#21569=CARTESIAN_POINT('',(14.,73.,14.));
#21570=CARTESIAN_POINT('',(0.,73.,14.));
#21571=CARTESIAN_POINT('',(14.,73.,-14.));
#21572=CARTESIAN_POINT('Origin',(14.,73.,0.));
#21573=CARTESIAN_POINT('',(0.,73.,-14.));
#21574=CARTESIAN_POINT('Origin',(0.,73.,14.));
#21575=CARTESIAN_POINT('',(14.,36.5,14.));
#21576=CARTESIAN_POINT('Origin',(14.,0.,0.));
#21577=CARTESIAN_POINT('Origin',(16.,0.,0.));
#21578=CARTESIAN_POINT('Origin',(14.,-30.4559107563704,12.));
#21579=CARTESIAN_POINT('',(14.,-73.,14.));
#21580=CARTESIAN_POINT('Origin',(14.,-73.,12.));
#21581=CARTESIAN_POINT('',(14.,-30.4559107563704,14.));
#21582=CARTESIAN_POINT('Origin',(14.,-73.,0.));
#21583=CARTESIAN_POINT('',(14.,-73.,-14.));
#21584=CARTESIAN_POINT('Origin',(14.,-73.,-12.));
#21585=CARTESIAN_POINT('Origin',(14.,-73.,0.));
#21586=CARTESIAN_POINT('Origin',(14.,-36.5,-12.));
#21587=CARTESIAN_POINT('',(14.,-36.5,-14.));
#21588=CARTESIAN_POINT('Origin',(0.,-73.,-14.));
#21589=CARTESIAN_POINT('',(0.,-73.,-14.));
#21590=CARTESIAN_POINT('Origin',(0.,-73.,0.));
#21591=CARTESIAN_POINT('',(0.,-73.,14.));
#21592=CARTESIAN_POINT('Origin',(0.,-60.9118215127409,14.));
#21593=CARTESIAN_POINT('Origin',(14.,0.,0.));
#21594=CARTESIAN_POINT('Origin',(16.,0.,0.));
#21595=CARTESIAN_POINT('Origin',(14.,30.4559107563704,-12.));
#21596=CARTESIAN_POINT('Origin',(14.,73.,-12.));
#21597=CARTESIAN_POINT('',(14.,30.4559107563704,-14.));
#21598=CARTESIAN_POINT('Origin',(14.,73.,0.));
#21599=CARTESIAN_POINT('Origin',(14.,73.,12.));
#21600=CARTESIAN_POINT('Origin',(14.,36.5,12.));
#21601=CARTESIAN_POINT('Origin',(0.,60.9118215127409,-14.));
#21602=CARTESIAN_POINT('Origin',(-8.17712434446771,0.,0.));
#21603=CARTESIAN_POINT('',(-8.17712434446771,-50.8,1.55887483312148E-14));
#21604=CARTESIAN_POINT('Origin',(-8.17712434446771,0.,0.));
#21605=CARTESIAN_POINT('',(-9.5,-50.3,1.54353157688997E-14));
#21606=CARTESIAN_POINT('Origin',(-8.17712434446771,-48.8,1.49750180819544E-14));
#21607=CARTESIAN_POINT('Origin',(-9.5,0.,0.));
#21608=CARTESIAN_POINT('Origin',(-4.45,0.,0.));
#21609=CARTESIAN_POINT('',(-4.45,-50.8,-6.22120573966855E-15));
#21610=CARTESIAN_POINT('Origin',(18.,16.,58.));
#21611=CARTESIAN_POINT('',(16.,-32.,58.));
#21612=CARTESIAN_POINT('',(16.,16.,58.));
#21613=CARTESIAN_POINT('Origin',(18.,-32.,58.));
#21614=CARTESIAN_POINT('Origin',(18.,-32.,32.));
#21615=CARTESIAN_POINT('',(16.,-58.,32.));
#21616=CARTESIAN_POINT('Origin',(18.,-58.,32.));
#21617=CARTESIAN_POINT('Origin',(18.,-32.,32.));
#21618=CARTESIAN_POINT('Origin',(16.,-32.,32.));
#21619=CARTESIAN_POINT('Origin',(18.,-58.,16.));
#21620=CARTESIAN_POINT('',(16.,-58.,16.));
#21621=CARTESIAN_POINT('Origin',(16.,0.,0.));
#21622=CARTESIAN_POINT('Origin',(18.,32.,32.));
#21623=CARTESIAN_POINT('',(16.,58.,32.));
#21624=CARTESIAN_POINT('Origin',(18.,58.,32.));
#21625=CARTESIAN_POINT('',(16.,32.,58.));
#21626=CARTESIAN_POINT('Origin',(16.,32.,32.));
#21627=CARTESIAN_POINT('Origin',(18.,32.,58.));
#21628=CARTESIAN_POINT('Origin',(18.,32.,32.));
#21629=CARTESIAN_POINT('Origin',(18.,16.,58.));
#21630=CARTESIAN_POINT('',(16.,16.,58.));
#21631=CARTESIAN_POINT('Origin',(18.,58.,-16.));
#21632=CARTESIAN_POINT('',(16.,58.,-16.));
#21633=CARTESIAN_POINT('Origin',(16.,0.,0.));
#21634=CARTESIAN_POINT('Origin',(18.,-16.,-58.));
#21635=CARTESIAN_POINT('',(16.,32.,-58.));
#21636=CARTESIAN_POINT('',(16.,-16.,-58.));
#21637=CARTESIAN_POINT('Origin',(18.,32.,-58.));
#21638=CARTESIAN_POINT('Origin',(18.,32.,-32.));
#21639=CARTESIAN_POINT('',(16.,58.,-32.));
#21640=CARTESIAN_POINT('Origin',(18.,58.,-32.));
#21641=CARTESIAN_POINT('Origin',(18.,32.,-32.));
#21642=CARTESIAN_POINT('Origin',(16.,32.,-32.));
#21643=CARTESIAN_POINT('Origin',(18.,58.,-16.));
#21644=CARTESIAN_POINT('',(16.,58.,-16.));
#21645=CARTESIAN_POINT('Origin',(16.,0.,0.));
#21646=CARTESIAN_POINT('Origin',(18.,-58.,16.));
#21647=CARTESIAN_POINT('',(16.,-58.,-32.));
#21648=CARTESIAN_POINT('',(16.,-58.,16.));
#21649=CARTESIAN_POINT('Origin',(18.,-58.,-32.));
#21650=CARTESIAN_POINT('Origin',(18.,-32.,-32.));
#21651=CARTESIAN_POINT('',(16.,-32.,-58.));
#21652=CARTESIAN_POINT('Origin',(18.,-32.,-58.));
#21653=CARTESIAN_POINT('Origin',(18.,-32.,-32.));
#21654=CARTESIAN_POINT('Origin',(16.,-32.,-32.));
#21655=CARTESIAN_POINT('Origin',(18.,-16.,-58.));
#21656=CARTESIAN_POINT('',(16.,-16.,-58.));
#21657=CARTESIAN_POINT('Origin',(16.,0.,0.));
#21658=CARTESIAN_POINT('Origin',(123.8,-16.,-58.));
#21659=CARTESIAN_POINT('Origin',(123.8,-32.,-58.));
#21660=CARTESIAN_POINT('Origin',(123.8,32.,-58.));
#21661=CARTESIAN_POINT('Origin',(123.8,32.,-32.));
#21662=CARTESIAN_POINT('Origin',(123.8,58.,-32.));
#21663=CARTESIAN_POINT('Origin',(123.8,32.,-32.));
#21664=CARTESIAN_POINT('Origin',(123.8,58.,-16.));
#21665=CARTESIAN_POINT('Origin',(123.8,58.,32.));
#21666=CARTESIAN_POINT('Origin',(123.8,32.,32.));
#21667=CARTESIAN_POINT('Origin',(123.8,32.,58.));
#21668=CARTESIAN_POINT('Origin',(123.8,32.,32.));
#21669=CARTESIAN_POINT('Origin',(123.8,16.,58.));
#21670=CARTESIAN_POINT('Origin',(123.8,-32.,58.));
#21671=CARTESIAN_POINT('Origin',(123.8,-32.,32.));
#21672=CARTESIAN_POINT('Origin',(123.8,-58.,32.));
#21673=CARTESIAN_POINT('Origin',(123.8,-32.,32.));
#21674=CARTESIAN_POINT('Origin',(123.8,-58.,16.));
#21675=CARTESIAN_POINT('Origin',(123.8,-58.,-32.));
#21676=CARTESIAN_POINT('Origin',(123.8,-32.,-32.));
#21677=CARTESIAN_POINT('Origin',(123.8,-32.,-32.));
#21678=CARTESIAN_POINT('Origin',(16.,32.,32.));
#21679=CARTESIAN_POINT('Origin',(16.,32.,-32.));
#21680=CARTESIAN_POINT('Origin',(123.8,0.,0.));
#21681=CARTESIAN_POINT('',(123.8,-6.12323399573677E-15,-50.));
#21682=CARTESIAN_POINT('Origin',(123.8,-6.36816335556624E-15,-52.));
#21683=CARTESIAN_POINT('',(123.8,-50.,6.12323399573677E-15));
#21684=CARTESIAN_POINT('Origin',(123.8,0.,0.));
#21685=CARTESIAN_POINT('Origin',(123.8,0.,0.));
#21686=CARTESIAN_POINT('Origin',(70.95,0.,0.));
#21687=CARTESIAN_POINT('',(16.,-50.,-6.12323399573677E-15));
#21688=CARTESIAN_POINT('Origin',(16.,0.,0.));
#21689=CARTESIAN_POINT('',(70.95,-50.,-6.12323399573677E-15));
#21690=CARTESIAN_POINT('',(71.6135123314049,23.3160685634306,44.2307692307674));
#21691=CARTESIAN_POINT('',(73.2907028363675,19.5959875136913,46.0001627885347));
#21692=CARTESIAN_POINT('Ctrl Pts',(71.6135123314072,23.3160685634275,44.2307692307691));
#21693=CARTESIAN_POINT('Ctrl Pts',(71.6932714543115,23.2042169236777,44.2897313638428));
#21694=CARTESIAN_POINT('Ctrl Pts',(71.8483990288815,22.9774859633438,44.4081667977607));
#21695=CARTESIAN_POINT('Ctrl Pts',(72.0309897669014,22.6869514584429,44.557072726346));
#21696=CARTESIAN_POINT('Ctrl Pts',(72.1700773346563,22.4505358369901,44.6764670164254));
#21697=CARTESIAN_POINT('Ctrl Pts',(72.3044475744177,22.211560601306,44.7959596617311));
#21698=CARTESIAN_POINT('Ctrl Pts',(72.4157517404387,21.9992281010938,44.9005387053819));
#21699=CARTESIAN_POINT('Ctrl Pts',(72.5065732598677,21.8151167092688,44.990045399374));
#21700=CARTESIAN_POINT('Ctrl Pts',(72.5658930280084,21.6918256295662,45.0496717620424));
#21701=CARTESIAN_POINT('Ctrl Pts',(72.6377280503905,21.5367060266982,45.1241021330032));
#21702=CARTESIAN_POINT('Ctrl Pts',(72.7201916785671,21.3490306679124,45.2131989345674));
#21703=CARTESIAN_POINT('Ctrl Pts',(72.7988814082159,21.1599111909158,45.302017540834));
#21704=CARTESIAN_POINT('Ctrl Pts',(72.8737703412485,20.969415619956,45.3905097941917));
#21705=CARTESIAN_POINT('Ctrl Pts',(72.9448178995343,20.7776647362872,45.4786056970811));
#21706=CARTESIAN_POINT('Ctrl Pts',(73.0121109467716,20.5844107113345,45.5664035981079));
#21707=CARTESIAN_POINT('Ctrl Pts',(73.0755852718533,20.3897951762557,45.6538223879631));
#21708=CARTESIAN_POINT('Ctrl Pts',(73.1352131070871,20.1938738237251,45.7408225076835));
#21709=CARTESIAN_POINT('Ctrl Pts',(73.1909498335265,19.9967609507555,45.8273396719058));
#21710=CARTESIAN_POINT('Ctrl Pts',(73.2341485984696,19.8314987172849,45.8990281581236));
#21711=CARTESIAN_POINT('Ctrl Pts',(73.2626675329748,19.7153221034526,45.9489756536103));
#21712=CARTESIAN_POINT('Ctrl Pts',(73.278471643703,19.6487953456216,45.977449084781));
#21713=CARTESIAN_POINT('Ctrl Pts',(73.2862090342068,19.6154867193585,45.9916623858903));
#21714=CARTESIAN_POINT('Ctrl Pts',(73.2902585153488,19.5978545384253,45.9991749778942));
#21715=CARTESIAN_POINT('Ctrl Pts',(73.2904803873088,19.5968878248965,45.9995868316516));
#21716=CARTESIAN_POINT('Ctrl Pts',(73.2907028377334,19.5959211154461,45.9999986482306));
#21717=CARTESIAN_POINT('',(53.3864876668068,23.3160685609229,44.2307692320894));
#21718=CARTESIAN_POINT('Ctrl Pts',(53.3864876668068,23.3160685609229,44.2307692320894));
#21719=CARTESIAN_POINT('Ctrl Pts',(53.8964899676441,24.0312794561666,43.8537487425402));
#21720=CARTESIAN_POINT('Ctrl Pts',(55.3186828044349,25.2435158958716,43.1695330127632));
#21721=CARTESIAN_POINT('Ctrl Pts',(58.0747486677894,26.2360703120526,42.564673612103));
#21722=CARTESIAN_POINT('Ctrl Pts',(61.020309894555,26.5481066493621,42.3696710366589));
#21723=CARTESIAN_POINT('Ctrl Pts',(63.9663874943631,26.5460492373018,42.3707472230138));
#21724=CARTESIAN_POINT('Ctrl Pts',(66.9244886027247,26.2356604580669,42.5652091566662));
#21725=CARTESIAN_POINT('Ctrl Pts',(69.681226557465,25.239555364586,43.1717497595138));
#21726=CARTESIAN_POINT('Ctrl Pts',(71.0985268893462,24.038267655457,43.8500649418989));
#21727=CARTESIAN_POINT('Ctrl Pts',(71.6135123314272,23.3160685633993,44.2307692307839));
#21728=CARTESIAN_POINT('',(51.7092971474407,19.5959037569241,45.9999667943664));
#21729=CARTESIAN_POINT('Ctrl Pts',(51.7092971610549,19.5959179422654,46.));
#21730=CARTESIAN_POINT('Ctrl Pts',(51.7312389779497,19.6914330268016,45.959302575355));
#21731=CARTESIAN_POINT('Ctrl Pts',(51.8239020992648,20.0709136872745,45.7962695577249));
#21732=CARTESIAN_POINT('Ctrl Pts',(52.0530341102106,20.8197959816443,45.4633470605684));
#21733=CARTESIAN_POINT('Ctrl Pts',(52.5423502486883,21.9908524941898,44.9125177602508));
#21734=CARTESIAN_POINT('Ctrl Pts',(53.0439951189989,22.8358340303902,44.4839588612342));
#21735=CARTESIAN_POINT('Ctrl Pts',(53.3864876668068,23.3160685609229,44.2307692320894));
#21736=CARTESIAN_POINT('Ctrl Pts',(73.2907028363675,19.5959875136913,46.0001627885347));
#21737=CARTESIAN_POINT('Ctrl Pts',(73.3614481346313,19.2876918400925,46.1319200512155));
#21738=CARTESIAN_POINT('Ctrl Pts',(73.4180753927526,18.9755505935139,46.2617120261331));
#21739=CARTESIAN_POINT('Ctrl Pts',(73.4601341604197,18.6605239219579,46.3888396110071));
#21740=CARTESIAN_POINT('Ctrl Pts',(73.4994000293548,18.3664164936491,46.5075253301233));
#21741=CARTESIAN_POINT('Ctrl Pts',(73.5260008275866,18.0698024364483,46.6238849103412));
#21742=CARTESIAN_POINT('Ctrl Pts',(73.5395273739608,17.7715244162219,46.737334373478));
#21743=CARTESIAN_POINT('Ctrl Pts',(73.5451949896521,17.6465460853884,46.784869637813));
#21744=CARTESIAN_POINT('Ctrl Pts',(73.5485678818421,17.521275662251,46.8318941375462));
#21745=CARTESIAN_POINT('Ctrl Pts',(73.5496186134852,17.395775144484,46.8783656049086));
#21746=CARTESIAN_POINT('Ctrl Pts',(73.550638568793,17.273950585317,46.9234759050572));
#21747=CARTESIAN_POINT('Ctrl Pts',(73.549470420523,17.1519092272119,46.9680651041026));
#21748=CARTESIAN_POINT('Ctrl Pts',(73.546122975365,17.0297456445921,47.0121211853996));
#21749=CARTESIAN_POINT('Ctrl Pts',(73.5385114955969,16.7519679384259,47.1122966791343));
#21750=CARTESIAN_POINT('Ctrl Pts',(73.5190626012108,16.473522026003,47.2097294454252));
#21751=CARTESIAN_POINT('Ctrl Pts',(73.488046964858,16.1953398787474,47.3043376488432));
#21752=CARTESIAN_POINT('Ctrl Pts',(73.4591781610324,15.9364128734918,47.3923972853989));
#21753=CARTESIAN_POINT('Ctrl Pts',(73.420288919625,15.6777138858939,47.4780101963045));
#21754=CARTESIAN_POINT('Ctrl Pts',(73.3715757825718,15.4199486044262,47.5611191306938));
#21755=CARTESIAN_POINT('Ctrl Pts',(73.3679532235023,15.4007798541739,47.5672995379154));
#21756=CARTESIAN_POINT('Ctrl Pts',(73.3642763241121,15.3816162471717,47.5734661006511));
#21757=CARTESIAN_POINT('Ctrl Pts',(73.3605451589308,15.3624580638881,47.5796187966842));
#21758=CARTESIAN_POINT('Ctrl Pts',(73.3071301487798,15.0881913121253,47.6677002149798));
#21759=CARTESIAN_POINT('Ctrl Pts',(73.2425888013964,14.8149979710872,47.7529521629476));
#21760=CARTESIAN_POINT('Ctrl Pts',(73.1668141764284,14.5438139588109,47.8352695279082));
#21761=CARTESIAN_POINT('Ctrl Pts',(73.0918525519906,14.2755395319778,47.9167036940224));
#21762=CARTESIAN_POINT('Ctrl Pts',(73.0058967816236,14.0092312159786,47.9952657482102));
#21763=CARTESIAN_POINT('Ctrl Pts',(72.9088264267727,13.7458407566761,48.0708394050032));
#21764=CARTESIAN_POINT('Ctrl Pts',(72.8316347408528,13.536389028185,48.130936619935));
#21765=CARTESIAN_POINT('Ctrl Pts',(72.7474141369172,13.3287833016545,48.1891437526931));
#21766=CARTESIAN_POINT('Ctrl Pts',(72.6561002844086,13.1235248126055,48.2453968530772));
#21767=CARTESIAN_POINT('Ctrl Pts',(72.5316712735188,12.8438289059336,48.3220502572211));
#21768=CARTESIAN_POINT('Ctrl Pts',(72.3946427652386,12.5682553157748,48.3951379950373));
#21769=CARTESIAN_POINT('Ctrl Pts',(72.245053609984,12.2981649671315,48.464464920355));
#21770=CARTESIAN_POINT('Ctrl Pts',(72.0983246196883,12.0332387826257,48.5324663054478));
#21771=CARTESIAN_POINT('Ctrl Pts',(71.939510779376,11.7735888662279,48.5968492518765));
#21772=CARTESIAN_POINT('Ctrl Pts',(71.7686966780188,11.5204923924152,48.6574411642038));
#21773=CARTESIAN_POINT('Ctrl Pts',(71.7001573486202,11.4189371785865,48.6817537297643));
#21774=CARTESIAN_POINT('Ctrl Pts',(71.6296864904025,11.3184369448846,48.705456067353));
#21775=CARTESIAN_POINT('Ctrl Pts',(71.5572917659591,11.2190734726146,48.7285376036628));
#21776=CARTESIAN_POINT('Ctrl Pts',(71.3768963941771,10.9714765564093,48.786052876439));
#21777=CARTESIAN_POINT('Ctrl Pts',(71.184552308396,10.7309398968218,48.8397126227416));
#21778=CARTESIAN_POINT('Ctrl Pts',(70.9813698482786,10.4983816308439,48.8897537967881));
#21779=CARTESIAN_POINT('Ctrl Pts',(70.7778012863261,10.2653814410245,48.9398900626508));
#21780=CARTESIAN_POINT('Ctrl Pts',(70.5633536284789,10.0403906456116,48.9863940944043));
#21781=CARTESIAN_POINT('Ctrl Pts',(70.3391832313088,9.8243010871711,49.0295155385523));
#21782=CARTESIAN_POINT('Ctrl Pts',(70.3154954232116,9.80146717128941,49.0340721281232));
#21783=CARTESIAN_POINT('Ctrl Pts',(70.2916990842856,9.77873261128666,49.0385909576319));
#21784=CARTESIAN_POINT('Ctrl Pts',(70.2677956009778,9.75609843423282,49.043072328228));
#21785=CARTESIAN_POINT('Ctrl Pts',(70.0118710660855,9.51376382715578,49.0910524770088));
#21786=CARTESIAN_POINT('Ctrl Pts',(69.7432342365535,9.28302248963847,49.1347219741822));
#21787=CARTESIAN_POINT('Ctrl Pts',(69.463336662313,9.06493981195789,49.1744863022742));
#21788=CARTESIAN_POINT('Ctrl Pts',(69.18146262429,8.84531716911266,49.2145314214896));
#21789=CARTESIAN_POINT('Ctrl Pts',(68.8881677361653,8.63853183864154,49.2506159507198));
#21790=CARTESIAN_POINT('Ctrl Pts',(68.5848877717148,8.44569449976274,49.2831415609367));
#21791=CARTESIAN_POINT('Ctrl Pts',(68.2845080196753,8.2547012300909,49.3153561345226));
#21792=CARTESIAN_POINT('Ctrl Pts',(67.9743325950966,8.07738978136323,49.3440794037022));
#21793=CARTESIAN_POINT('Ctrl Pts',(67.6557196810578,7.91487194608282,49.3696909984755));
#21794=CARTESIAN_POINT('Ctrl Pts',(67.3613870476161,7.76473897804652,49.3933508308431));
#21795=CARTESIAN_POINT('Ctrl Pts',(67.0598531374047,7.62723068755149,49.414354985105));
#21796=CARTESIAN_POINT('Ctrl Pts',(66.7521676869351,7.50325643845802,49.4329960508709));
#21797=CARTESIAN_POINT('Ctrl Pts',(66.50225675491,7.40256100391349,49.448136858187));
#21798=CARTESIAN_POINT('Ctrl Pts',(66.2484614297923,7.31061703715261,49.4617452712725));
#21799=CARTESIAN_POINT('Ctrl Pts',(65.9913615551387,7.2279790305136,49.4739653333684));
#21800=CARTESIAN_POINT('Ctrl Pts',(65.6570871797071,7.12053530618906,49.4898535310205));
#21801=CARTESIAN_POINT('Ctrl Pts',(65.3172247744756,7.02882321195569,49.5033947318101));
#21802=CARTESIAN_POINT('Ctrl Pts',(64.9734117791745,6.95299333693358,49.5145694818844));
#21803=CARTESIAN_POINT('Ctrl Pts',(64.6278849499738,6.87678546627959,49.5257999356865));
#21804=CARTESIAN_POINT('Ctrl Pts',(64.2783681408376,6.81661934572417,49.5346403474515));
#21805=CARTESIAN_POINT('Ctrl Pts',(63.9265760227067,6.7726460431142,49.5410742954058));
#21806=CARTESIAN_POINT('Ctrl Pts',(63.5742519227226,6.72860624384951,49.5475179728092));
#21807=CARTESIAN_POINT('Ctrl Pts',(63.2196458701498,6.70080908424267,49.5515479323014));
#21808=CARTESIAN_POINT('Ctrl Pts',(62.8645303999073,6.68939242925534,49.5531503258018));
#21809=CARTESIAN_POINT('Ctrl Pts',(62.7430551295141,6.6854871044588,49.5536984607045));
#21810=CARTESIAN_POINT('Ctrl Pts',(62.6215206631554,6.68349834754966,49.5539625582977));
#21811=CARTESIAN_POINT('Ctrl Pts',(62.499999199999,6.6834310420419,49.5539421295715));
#21812=CARTESIAN_POINT('Ctrl Pts',(62.1897600464977,6.68325921392849,49.553889975898));
#21813=CARTESIAN_POINT('Ctrl Pts',(61.8794936145935,6.69574259278768,49.5519656432217));
#21814=CARTESIAN_POINT('Ctrl Pts',(61.5703573069878,6.7207420019746,49.5481895211902));
#21815=CARTESIAN_POINT('Ctrl Pts',(61.2608873346803,6.74576839414671,49.5444093234207));
#21816=CARTESIAN_POINT('Ctrl Pts',(60.9525498130144,6.78333706171612,49.5387733420942));
#21817=CARTESIAN_POINT('Ctrl Pts',(60.6464542896073,6.83331469294025,49.5313004859268));
#21818=CARTESIAN_POINT('Ctrl Pts',(60.523559121281,6.85338035523245,49.5283001875025));
#21819=CARTESIAN_POINT('Ctrl Pts',(60.4010247844408,6.87544643607457,49.5250037737621));
#21820=CARTESIAN_POINT('Ctrl Pts',(60.2789208350937,6.89950503634368,49.5214124066634));
#21821=CARTESIAN_POINT('Ctrl Pts',(59.9277856936677,6.96869051357988,49.5110846883473));
#21822=CARTESIAN_POINT('Ctrl Pts',(59.5801503156904,7.05408058719238,49.4983547685931));
#21823=CARTESIAN_POINT('Ctrl Pts',(59.2378514600242,7.15571464542734,49.4832256563387));
#21824=CARTESIAN_POINT('Ctrl Pts',(59.1609163729305,7.1785579152559,49.4798252372322));
#21825=CARTESIAN_POINT('Ctrl Pts',(59.0842508602296,7.20222158226451,49.4763036692557));
#21826=CARTESIAN_POINT('Ctrl Pts',(59.0078757360508,7.22670573976275,49.4726610750435));
#21827=CARTESIAN_POINT('Ctrl Pts',(58.6908785430507,7.32832795358386,49.4575423809281));
#21828=CARTESIAN_POINT('Ctrl Pts',(58.3788847972949,7.44408741355368,49.4403379670896));
#21829=CARTESIAN_POINT('Ctrl Pts',(58.0730988777378,7.5729945695746,49.4207696740327));
#21830=CARTESIAN_POINT('Ctrl Pts',(57.74966674389,7.70934066621787,49.4000721390112));
#21831=CARTESIAN_POINT('Ctrl Pts',(57.4334521150688,7.8608904174952,49.3766553872395));
#21832=CARTESIAN_POINT('Ctrl Pts',(57.1256864306589,8.02646056782285,49.3501805334311));
#21833=CARTESIAN_POINT('Ctrl Pts',(56.814041913381,8.19411743208113,49.3233720117114));
#21834=CARTESIAN_POINT('Ctrl Pts',(56.5110598816884,8.37615053289667,49.2934279876878));
#21835=CARTESIAN_POINT('Ctrl Pts',(56.218019637168,8.57138477273958,49.2599889073673));
#21836=CARTESIAN_POINT('Ctrl Pts',(55.9242821674943,8.76708352974473,49.2264702660706));
#21837=CARTESIAN_POINT('Ctrl Pts',(55.6405329777448,8.9760466670762,49.1894401167517));
#21838=CARTESIAN_POINT('Ctrl Pts',(55.3680736173629,9.19713973768636,49.148525887908));
#21839=CARTESIAN_POINT('Ctrl Pts',(55.2153011969308,9.32111023916053,49.1255846104939));
#21840=CARTESIAN_POINT('Ctrl Pts',(55.0660786369272,9.44889527856915,49.1014219643564));
#21841=CARTESIAN_POINT('Ctrl Pts',(54.9206388099483,9.58030092990195,49.0759704510606));
#21842=CARTESIAN_POINT('Ctrl Pts',(54.6873329934736,9.79109396651661,49.0351426653478));
#21843=CARTESIAN_POINT('Ctrl Pts',(54.4635724344831,10.0113464810153,48.9909702843494));
#21844=CARTESIAN_POINT('Ctrl Pts',(54.2505163116649,10.2400992217127,48.9431994614762));
#21845=CARTESIAN_POINT('Ctrl Pts',(54.0371783773243,10.4691545360102,48.8953654516448));
#21846=CARTESIAN_POINT('Ctrl Pts',(53.8345735518,10.7067318313352,48.8439234119285));
#21847=CARTESIAN_POINT('Ctrl Pts',(53.6438198607322,10.9518453411613,48.7886281792624));
#21848=CARTESIAN_POINT('Ctrl Pts',(53.5751826699505,11.0400423382571,48.7687317913468));
#21849=CARTESIAN_POINT('Ctrl Pts',(53.5080794064406,11.1292148992273,48.7483366211777));
#21850=CARTESIAN_POINT('Ctrl Pts',(53.4425605926292,11.2193166643701,48.7274315729019));
#21851=CARTESIAN_POINT('Ctrl Pts',(53.2598511346751,11.4705795263217,48.6691345767143));
#21852=CARTESIAN_POINT('Ctrl Pts',(53.0894670854084,11.7290686403632,48.6068717193985));
#21853=CARTESIAN_POINT('Ctrl Pts',(52.9314780004343,11.9934610506509,48.5408180490906));
#21854=CARTESIAN_POINT('Ctrl Pts',(52.7697206955817,12.2641595214891,48.4731889234052));
#21855=CARTESIAN_POINT('Ctrl Pts',(52.6209565156028,12.5410454414813,48.4015861388442));
#21856=CARTESIAN_POINT('Ctrl Pts',(52.4852071420199,12.8227024785657,48.3262070143474));
#21857=CARTESIAN_POINT('Ctrl Pts',(52.4676741301488,12.8590805188059,48.3164712560913));
#21858=CARTESIAN_POINT('Ctrl Pts',(52.4503581571292,12.8955381632686,48.3066725134332));
#21859=CARTESIAN_POINT('Ctrl Pts',(52.4332592094338,12.9320723751521,48.2968112208205));
#21860=CARTESIAN_POINT('Ctrl Pts',(52.3034526058899,13.2094217209856,48.221949251335));
#21861=CARTESIAN_POINT('Ctrl Pts',(52.1866217579404,13.4913117239867,48.1434486683242));
#21862=CARTESIAN_POINT('Ctrl Pts',(52.0826632708201,13.7765258626941,48.0614627034639));
#21863=CARTESIAN_POINT('Ctrl Pts',(51.9773786777555,14.0653782244576,47.9784309165802));
#21864=CARTESIAN_POINT('Ctrl Pts',(51.8852963255834,14.3576403533906,47.891824431865));
#21865=CARTESIAN_POINT('Ctrl Pts',(51.8063250046279,14.6520979265174,47.8017885914336));
#21866=CARTESIAN_POINT('Ctrl Pts',(51.7541270394914,14.8467266341326,47.7422772700703));
#21867=CARTESIAN_POINT('Ctrl Pts',(51.707657455628,15.042315526251,47.6812674158652));
#21868=CARTESIAN_POINT('Ctrl Pts',(51.6668956843904,15.2385243562794,47.6187972727124));
#21869=CARTESIAN_POINT('Ctrl Pts',(51.6071148687816,15.5262823101803,47.5271791708618));
#21870=CARTESIAN_POINT('Ctrl Pts',(51.5595992934775,15.8154197044411,47.4324063334734));
#21871=CARTESIAN_POINT('Ctrl Pts',(51.5244938097377,16.1049522263608,47.3345616995291));
#21872=CARTESIAN_POINT('Ctrl Pts',(51.4914040437863,16.3778601132494,47.2423351955216));
#21873=CARTESIAN_POINT('Ctrl Pts',(51.4693408708349,16.6511190964164,47.14737936348));
#21874=CARTESIAN_POINT('Ctrl Pts',(51.4584591192422,16.9238788974805,47.0497630002213));
#21875=CARTESIAN_POINT('Ctrl Pts',(51.4521604547632,17.0817599569435,46.9932598982535));
#21876=CARTESIAN_POINT('Ctrl Pts',(51.4496040028725,17.2394928872624,46.9358582204704));
#21877=CARTESIAN_POINT('Ctrl Pts',(51.4507739583774,17.3968661691267,46.8775869639482));
#21878=CARTESIAN_POINT('Ctrl Pts',(51.4528052320093,17.6700972420113,46.7764165635518));
#21879=CARTESIAN_POINT('Ctrl Pts',(51.4660705043716,17.942241477422,46.6726253927475));
#21880=CARTESIAN_POINT('Ctrl Pts',(51.4900980818398,18.2126518952105,46.5666544818487));
#21881=CARTESIAN_POINT('Ctrl Pts',(51.499926823275,18.3232662125019,46.5233059302001));
#21882=CARTESIAN_POINT('Ctrl Pts',(51.5115561621439,18.4335909686908,46.4795925387909));
#21883=CARTESIAN_POINT('Ctrl Pts',(51.5249529285916,18.5435841236212,46.4355440051706));
#21884=CARTESIAN_POINT('Ctrl Pts',(51.5638198253953,18.8626978902522,46.3077497484552));
#21885=CARTESIAN_POINT('Ctrl Pts',(51.6176238310752,19.1789902861077,46.17714612138));
#21886=CARTESIAN_POINT('Ctrl Pts',(51.6859043886847,19.4914647591776,46.0444546103236));
#21887=CARTESIAN_POINT('Ctrl Pts',(51.6935220631743,19.52632576362,46.0296509711305));
#21888=CARTESIAN_POINT('Ctrl Pts',(51.7013198745586,19.5611392285382,46.0148213612344));
#21889=CARTESIAN_POINT('Ctrl Pts',(51.7092971474407,19.5959037569241,45.9999667943664));
#21890=CARTESIAN_POINT('',(53.3864876685947,23.3160685634302,-44.2307692307677));
#21891=CARTESIAN_POINT('',(51.7092971560459,19.59597217608,-46.0001268989906));
#21892=CARTESIAN_POINT('Ctrl Pts',(53.3864876685928,23.3160685634274,-44.2307692307691));
#21893=CARTESIAN_POINT('Ctrl Pts',(52.930215177034,22.6766294615115,-44.5679874350866));
#21894=CARTESIAN_POINT('Ctrl Pts',(52.3546179283007,21.6420362564594,-45.0860447448006));
#21895=CARTESIAN_POINT('Ctrl Pts',(51.9005239862315,20.3541704296053,-45.6727447106325));
#21896=CARTESIAN_POINT('Ctrl Pts',(51.7529482282219,19.7864858334401,-45.9188374584652));
#21897=CARTESIAN_POINT('Ctrl Pts',(51.7092971610549,19.5959179422654,-46.));
#21898=CARTESIAN_POINT('',(71.6135123331932,23.3160685609228,-44.2307692320894));
#21899=CARTESIAN_POINT('Ctrl Pts',(71.6135123331932,23.3160685609229,-44.2307692320894));
#21900=CARTESIAN_POINT('Ctrl Pts',(71.1035100323559,24.0312794561666,-43.8537487425401));
#21901=CARTESIAN_POINT('Ctrl Pts',(69.681000122088,25.243380770632,-43.1696388054261));
#21902=CARTESIAN_POINT('Ctrl Pts',(66.9248798545188,26.2358932678842,-42.5648089417427));
#21903=CARTESIAN_POINT('Ctrl Pts',(63.9785719433368,26.5476372801886,-42.3700397756168));
#21904=CARTESIAN_POINT('Ctrl Pts',(61.0328912216257,26.5456758334602,-42.3710278989254));
#21905=CARTESIAN_POINT('Ctrl Pts',(58.0708968314258,26.2337622543912,-42.5667104493236));
#21906=CARTESIAN_POINT('Ctrl Pts',(55.3220849100951,25.2411372376895,-43.1704876695772));
#21907=CARTESIAN_POINT('Ctrl Pts',(53.9014731106537,24.038267655457,-43.8500649418989));
#21908=CARTESIAN_POINT('Ctrl Pts',(53.3864876685727,23.3160685633993,-44.2307692307839));
#21909=CARTESIAN_POINT('',(73.2907034369536,19.5966777272658,-46.0017752735852));
#21910=CARTESIAN_POINT('Ctrl Pts',(73.2907028389451,19.5959179422654,-46.));
#21911=CARTESIAN_POINT('Ctrl Pts',(73.2470092805887,19.7866035098537,-45.918783509084));
#21912=CARTESIAN_POINT('Ctrl Pts',(73.099528966838,20.3540492246571,-45.6728025929409));
#21913=CARTESIAN_POINT('Ctrl Pts',(72.6451832973973,21.6425621324406,-45.085801261871));
#21914=CARTESIAN_POINT('Ctrl Pts',(72.0694661900611,22.6771055141269,-44.5677393482618));
#21915=CARTESIAN_POINT('Ctrl Pts',(71.6135123331932,23.3160685609229,-44.2307692320894));
#21916=CARTESIAN_POINT('Ctrl Pts',(51.7092971560459,19.59597217608,-46.0001268989906));
#21917=CARTESIAN_POINT('Ctrl Pts',(51.6385518403573,19.2876757489281,-46.1318817425142));
#21918=CARTESIAN_POINT('Ctrl Pts',(51.5819245584145,18.9755341558142,-46.2616720942883));
#21919=CARTESIAN_POINT('Ctrl Pts',(51.5398657706017,18.6605076764483,-46.3887993378678));
#21920=CARTESIAN_POINT('Ctrl Pts',(51.5006578079912,18.3668342952929,-46.5073096533628));
#21921=CARTESIAN_POINT('Ctrl Pts',(51.4740774632621,18.0706621527521,-46.6235017985892));
#21922=CARTESIAN_POINT('Ctrl Pts',(51.4605290511144,17.7728302731532,-46.7367947468215));
#21923=CARTESIAN_POINT('Ctrl Pts',(51.4548236966847,17.6474106730525,-46.7845033946689));
#21924=CARTESIAN_POINT('Ctrl Pts',(51.4514287239645,17.5216967680026,-46.831698062969));
#21925=CARTESIAN_POINT('Ctrl Pts',(51.4503716252683,17.395751159985,-46.878336081621));
#21926=CARTESIAN_POINT('Ctrl Pts',(51.4493491529656,17.2739310344796,-46.9234464223063));
#21927=CARTESIAN_POINT('Ctrl Pts',(51.450513887619,17.1518941504805,-46.9680359923664));
#21928=CARTESIAN_POINT('Ctrl Pts',(51.4538566793357,17.0297349131611,-47.0120927720276));
#21929=CARTESIAN_POINT('Ctrl Pts',(51.4614578177917,16.7519583254358,-47.1122730137268));
#21930=CARTESIAN_POINT('Ctrl Pts',(51.4809069176557,16.4735134961054,-47.2097118040983));
#21931=CARTESIAN_POINT('Ctrl Pts',(51.5119283016989,16.1953334611301,-47.3043262340131));
#21932=CARTESIAN_POINT('Ctrl Pts',(51.540698040569,15.9373447474744,-47.3920732035939));
#21933=CARTESIAN_POINT('Ctrl Pts',(51.5794206384715,15.6795832662395,-47.4773912990985));
#21934=CARTESIAN_POINT('Ctrl Pts',(51.6278972920848,15.4227471168001,-47.560223409641));
#21935=CARTESIAN_POINT('Ctrl Pts',(51.6316912863093,15.4026460001803,-47.5667062116824));
#21936=CARTESIAN_POINT('Ctrl Pts',(51.6355450406446,15.3825505288608,-47.5731737896757));
#21937=CARTESIAN_POINT('Ctrl Pts',(51.6394584670014,15.3624610260131,-47.5796261178597));
#21938=CARTESIAN_POINT('Ctrl Pts',(51.6930034559185,15.0875888017152,-47.6679093279152));
#21939=CARTESIAN_POINT('Ctrl Pts',(51.7577243091049,14.8137957347893,-47.7533501196269));
#21940=CARTESIAN_POINT('Ctrl Pts',(51.8337259645455,14.5420228082065,-47.8358424485127));
#21941=CARTESIAN_POINT('Ctrl Pts',(51.9089081757662,14.2731801171894,-47.9174453512183));
#21942=CARTESIAN_POINT('Ctrl Pts',(51.9951298650042,14.0063139027635,-47.996162867403));
#21943=CARTESIAN_POINT('Ctrl Pts',(52.0925098200243,13.7423805361162,-48.0718777857805));
#21944=CARTESIAN_POINT('Ctrl Pts',(52.1693510364042,13.5341142565495,-48.1316234123319));
#21945=CARTESIAN_POINT('Ctrl Pts',(52.2531404764403,13.3276749982247,-48.1894991234461));
#21946=CARTESIAN_POINT('Ctrl Pts',(52.3439403254426,13.123554663829,-48.2454419686112));
#21947=CARTESIAN_POINT('Ctrl Pts',(52.4684627414818,12.8436251542427,-48.3221616803357));
#21948=CARTESIAN_POINT('Ctrl Pts',(52.6056097228968,12.5678248642511,-48.3953077688502));
#21949=CARTESIAN_POINT('Ctrl Pts',(52.7553388941879,12.2975172107946,-48.4646841952477));
#21950=CARTESIAN_POINT('Ctrl Pts',(52.9022559211048,12.0322863512615,-48.5327576255389));
#21951=CARTESIAN_POINT('Ctrl Pts',(53.0612868734049,11.7723444464564,-48.597201600181));
#21952=CARTESIAN_POINT('Ctrl Pts',(53.2323438982412,11.5189716531332,-48.6578426352013));
#21953=CARTESIAN_POINT('Ctrl Pts',(53.3005491093911,11.4179448471029,-48.6820219087615));
#21954=CARTESIAN_POINT('Ctrl Pts',(53.3706657391247,11.3179622781613,-48.7055967135365));
#21955=CARTESIAN_POINT('Ctrl Pts',(53.442686077265,11.2191043549872,-48.7285566222298));
#21956=CARTESIAN_POINT('Ctrl Pts',(53.6327962249655,10.9581517565786,-48.7891632750948));
#21957=CARTESIAN_POINT('Ctrl Pts',(53.8361749008966,10.7050379372868,-48.8454843564192));
#21958=CARTESIAN_POINT('Ctrl Pts',(54.0515222172661,10.4608362127091,-48.8977992033643));
#21959=CARTESIAN_POINT('Ctrl Pts',(54.2668695336356,10.2166344881313,-48.9501140503093));
#21960=CARTESIAN_POINT('Ctrl Pts',(54.4941848042496,9.98134567167982,-48.9984228060815));
#21961=CARTESIAN_POINT('Ctrl Pts',(54.7321208981018,9.75600333679323,-49.0430185827488));
#21962=CARTESIAN_POINT('Ctrl Pts',(54.9899860177656,9.51178680280687,-49.0913496076919));
#21963=CARTESIAN_POINT('Ctrl Pts',(55.2607617392154,9.27933854335903,-49.1353032978477));
#21964=CARTESIAN_POINT('Ctrl Pts',(55.5429655559212,9.05975496159557,-49.175295155659));
#21965=CARTESIAN_POINT('Ctrl Pts',(55.8271714636345,8.83861354720046,-49.215570735143));
#21966=CARTESIAN_POINT('Ctrl Pts',(56.1229687184755,8.63051923627181,-49.2518279919302));
#21967=CARTESIAN_POINT('Ctrl Pts',(56.4288895222584,8.43661493297673,-49.2844787968497));
#21968=CARTESIAN_POINT('Ctrl Pts',(56.7317789105064,8.24463205676346,-49.3168060600027));
#21969=CARTESIAN_POINT('Ctrl Pts',(57.0445928756025,8.06655867848375,-49.3455978623814));
#21970=CARTESIAN_POINT('Ctrl Pts',(57.3659431504788,7.90353716984582,-49.3712432917112));
#21971=CARTESIAN_POINT('Ctrl Pts',(57.6533784626551,7.75772077605303,-49.3941821299871));
#21972=CARTESIAN_POINT('Ctrl Pts',(57.9476441343405,7.6239468622901,-49.4146034724474));
#21973=CARTESIAN_POINT('Ctrl Pts',(58.2477651166754,7.50306255228726,-49.4327797488888));
#21974=CARTESIAN_POINT('Ctrl Pts',(58.4975711794082,7.40244435061056,-49.4479087945744));
#21975=CARTESIAN_POINT('Ctrl Pts',(58.7512496391542,7.31056607104857,-49.4615109231862));
#21976=CARTESIAN_POINT('Ctrl Pts',(59.008227698853,7.22798170126681,-49.4737304827943));
#21977=CARTESIAN_POINT('Ctrl Pts',(59.3398348334007,7.12141398006192,-49.4894987283474));
#21978=CARTESIAN_POINT('Ctrl Pts',(59.6769381471779,7.03032234664094,-49.5029647272155));
#21979=CARTESIAN_POINT('Ctrl Pts',(60.0179418759644,6.95485237030223,-49.5141055813766));
#21980=CARTESIAN_POINT('Ctrl Pts',(60.3605801711652,6.87902063636911,-49.52529983808));
#21981=CARTESIAN_POINT('Ctrl Pts',(60.7071563180931,6.81896148438955,-49.5341466700947));
#21982=CARTESIAN_POINT('Ctrl Pts',(61.0559988496054,6.7748238911007,-49.5406258175578));
#21983=CARTESIAN_POINT('Ctrl Pts',(61.4054206812244,6.73061300138095,-49.5471157245197));
#21984=CARTESIAN_POINT('Ctrl Pts',(61.7571162374109,6.70237741219055,-49.5512301065058));
#21985=CARTESIAN_POINT('Ctrl Pts',(62.1093548494777,6.69025593610002,-49.5529508633559));
#21986=CARTESIAN_POINT('Ctrl Pts',(62.2395261290315,6.68577639297575,-49.5535867763799));
#21987=CARTESIAN_POINT('Ctrl Pts',(62.3697710905136,6.68349739089685,-49.5538958114346));
#21988=CARTESIAN_POINT('Ctrl Pts',(62.5000007333252,6.6834252155456,-49.553877126063));
#21989=CARTESIAN_POINT('Ctrl Pts',(62.8097155764128,6.68325356662524,-49.5538326881239));
#21990=CARTESIAN_POINT('Ctrl Pts',(63.1194577152876,6.69569491589049,-49.5519170125618));
#21991=CARTESIAN_POINT('Ctrl Pts',(63.4280754364061,6.72060885415301,-49.5481478701364));
#21992=CARTESIAN_POINT('Ctrl Pts',(63.7370397386601,6.74555077104548,-49.5443744949221));
#21993=CARTESIAN_POINT('Ctrl Pts',(64.0448772410107,6.78299251361625,-49.5387434959438));
#21994=CARTESIAN_POINT('Ctrl Pts',(64.3504836874022,6.8328013328013,-49.531270901804));
#21995=CARTESIAN_POINT('Ctrl Pts',(64.4744054403698,6.85299853825798,-49.5282408054957));
#21996=CARTESIAN_POINT('Ctrl Pts',(64.5979609246064,6.87522937050882,-49.5249078823961));
#21997=CARTESIAN_POINT('Ctrl Pts',(64.7210788121852,6.89948581992488,-49.5212731237058));
#21998=CARTESIAN_POINT('Ctrl Pts',(65.0660710748529,6.96745553198623,-49.511088059216));
#21999=CARTESIAN_POINT('Ctrl Pts',(65.4076926497551,7.05106731795702,-49.4985686629476));
#22000=CARTESIAN_POINT('Ctrl Pts',(65.7441803838235,7.15037661535603,-49.4837109986881));
#22001=CARTESIAN_POINT('Ctrl Pts',(65.8269025362683,7.17479081536061,-49.4800583901576));
#22002=CARTESIAN_POINT('Ctrl Pts',(65.9093143931007,7.20015349248548,-49.4762645202421));
#22003=CARTESIAN_POINT('Ctrl Pts',(65.991389748064,7.2264649962254,-49.4723294411694));
#22004=CARTESIAN_POINT('Ctrl Pts',(66.3086238569636,7.32816308143608,-49.4571197438902));
#22005=CARTESIAN_POINT('Ctrl Pts',(66.6208301978817,7.44403920999634,-49.4397996750938));
#22006=CARTESIAN_POINT('Ctrl Pts',(66.926800548608,7.5731204565235,-49.420095339914));
#22007=CARTESIAN_POINT('Ctrl Pts',(67.2504549652406,7.70966216863315,-49.3992521598719));
#22008=CARTESIAN_POINT('Ctrl Pts',(67.5668631764223,7.86143247699165,-49.3756727657487));
#22009=CARTESIAN_POINT('Ctrl Pts',(67.874803872692,8.02722773016472,-49.3490305978458));
#22010=CARTESIAN_POINT('Ctrl Pts',(68.1861814260509,8.19487338699715,-49.3220910826785));
#22011=CARTESIAN_POINT('Ctrl Pts',(68.4889021298989,8.37685882175698,-49.2920202104801));
#22012=CARTESIAN_POINT('Ctrl Pts',(68.7817131552383,8.5719921786175,-49.258474106054));
#22013=CARTESIAN_POINT('Ctrl Pts',(69.0759255823596,8.7680594491983,-49.2247674490311));
#22014=CARTESIAN_POINT('Ctrl Pts',(69.3601341337972,8.97740094285658,-49.1875524295181));
#22015=CARTESIAN_POINT('Ctrl Pts',(69.6330655668965,9.19885896783842,-49.1464710786446));
#22016=CARTESIAN_POINT('Ctrl Pts',(69.7852554420347,9.32234664673131,-49.1235636194745));
#22017=CARTESIAN_POINT('Ctrl Pts',(69.9339387945752,9.44960263907514,-49.0994538173633));
#22018=CARTESIAN_POINT('Ctrl Pts',(70.0788929097391,9.58043280330667,-49.074077970154));
#22019=CARTESIAN_POINT('Ctrl Pts',(70.313741452996,9.79239831700799,-49.0329650928528));
#22020=CARTESIAN_POINT('Ctrl Pts',(70.5388860635807,10.0139710221455,-48.9884846155056));
#22021=CARTESIAN_POINT('Ctrl Pts',(70.753167983785,10.2441724186941,-48.940386756241));
#22022=CARTESIAN_POINT('Ctrl Pts',(70.9671407044207,10.4740416445564,-48.8923583001127));
#22023=CARTESIAN_POINT('Ctrl Pts',(71.1702817452254,10.7125139494238,-48.8407228352381));
#22024=CARTESIAN_POINT('Ctrl Pts',(71.3614834897188,10.9585938930529,-48.7852416133112));
#22025=CARTESIAN_POINT('Ctrl Pts',(71.4277417106301,11.0438693664019,-48.7660153919783));
#22026=CARTESIAN_POINT('Ctrl Pts',(71.4925666055447,11.130058281564,-48.7463274369041));
#22027=CARTESIAN_POINT('Ctrl Pts',(71.5559134725786,11.2171188605618,-48.7261681080344));
#22028=CARTESIAN_POINT('Ctrl Pts',(71.7401164260449,11.4702776438259,-48.6675478779967));
#22029=CARTESIAN_POINT('Ctrl Pts',(71.9118180082778,11.7308069507897,-48.6049411772279));
#22030=CARTESIAN_POINT('Ctrl Pts',(72.0709262012242,11.9973397782098,-48.5385160452646));
#22031=CARTESIAN_POINT('Ctrl Pts',(72.2333720073538,12.2694636657889,-48.4706975130492));
#22032=CARTESIAN_POINT('Ctrl Pts',(72.382690706961,12.5478447668155,-48.3988988215467));
#22033=CARTESIAN_POINT('Ctrl Pts',(72.5188369630493,12.8310332930558,-48.3233079989623));
#22034=CARTESIAN_POINT('Ctrl Pts',(72.5349764975393,12.8646040361503,-48.3143470423905));
#22035=CARTESIAN_POINT('Ctrl Pts',(72.5509309767563,12.8982423522582,-48.3053328036926));
#22036=CARTESIAN_POINT('Ctrl Pts',(72.5667003710721,12.9319458389031,-48.2962656029511));
#22037=CARTESIAN_POINT('Ctrl Pts',(72.7016360439085,13.2203400889478,-48.2186793109041));
#22038=CARTESIAN_POINT('Ctrl Pts',(72.8227250989957,13.5135818270332,-48.1371954523817));
#22039=CARTESIAN_POINT('Ctrl Pts',(72.9300166259904,13.8103594828784,-48.0519571049851));
#22040=CARTESIAN_POINT('Ctrl Pts',(73.0392119181037,14.1124031179207,-47.9652063008542));
#22041=CARTESIAN_POINT('Ctrl Pts',(73.1341161579519,14.4181097938983,-47.8745666597572));
#22042=CARTESIAN_POINT('Ctrl Pts',(73.2147473606732,14.726136307171,-47.7801737084575));
#22043=CARTESIAN_POINT('Ctrl Pts',(73.2592937260174,14.8963118860146,-47.7280243822338));
#22044=CARTESIAN_POINT('Ctrl Pts',(73.2994829882609,15.0671961837113,-47.6747291808002));
#22045=CARTESIAN_POINT('Ctrl Pts',(73.3353131082983,15.238566723947,-47.6203089053636));
#22046=CARTESIAN_POINT('Ctrl Pts',(73.4041812486989,15.5679535753776,-47.5157091115167));
#22047=CARTESIAN_POINT('Ctrl Pts',(73.4565608204754,15.8992610194355,-47.4069137146754));
#22048=CARTESIAN_POINT('Ctrl Pts',(73.4923097438172,16.2308818128794,-47.2940631567242));
#22049=CARTESIAN_POINT('Ctrl Pts',(73.5172428346201,16.4621707743967,-47.2153555217652));
#22050=CARTESIAN_POINT('Ctrl Pts',(73.534085099451,16.693612313661,-47.134675100752));
#22051=CARTESIAN_POINT('Ctrl Pts',(73.5427735626241,16.9246603998039,-47.0520669694327));
#22052=CARTESIAN_POINT('Ctrl Pts',(73.5487224225862,17.0828555468144,-46.9955064252772));
#22053=CARTESIAN_POINT('Ctrl Pts',(73.55102694222,17.2408810307338,-46.9380367751146));
#22054=CARTESIAN_POINT('Ctrl Pts',(73.5496650158222,17.3985337770098,-46.8796814170754));
#22055=CARTESIAN_POINT('Ctrl Pts',(73.5470374585348,17.7026923739799,-46.7670967381138));
#22056=CARTESIAN_POINT('Ctrl Pts',(73.5307595350488,18.005463438459,-46.6512144067101));
#22057=CARTESIAN_POINT('Ctrl Pts',(73.5012734326613,18.3059881853662,-46.5326475787612));
#22058=CARTESIAN_POINT('Ctrl Pts',(73.4934571778605,18.3856520882075,-46.501217567226));
#22059=CARTESIAN_POINT('Ctrl Pts',(73.4847130769512,18.4651581483415,-46.4695989899252));
#22060=CARTESIAN_POINT('Ctrl Pts',(73.4750499542682,18.5444903963155,-46.4378034063969));
#22061=CARTESIAN_POINT('Ctrl Pts',(73.4381093912684,18.8477648139483,-46.3162540072046));
#22062=CARTESIAN_POINT('Ctrl Pts',(73.3876764007721,19.1484717215781,-46.1921283391257));
#22063=CARTESIAN_POINT('Ctrl Pts',(73.3241452988119,19.4457621095765,-46.0660620702451));
#22064=CARTESIAN_POINT('Ctrl Pts',(73.3133737523194,19.4961669843122,-46.0446878356655));
#22065=CARTESIAN_POINT('Ctrl Pts',(73.3022257825704,19.5464735904137,-46.0232578551976));
#22066=CARTESIAN_POINT('Ctrl Pts',(73.2907034369536,19.5966777272658,-46.0017752735852));
#22067=CARTESIAN_POINT('Ctrl Pts',(55.0359921611649,23.1177228316711,46.));
#22068=CARTESIAN_POINT('Ctrl Pts',(54.6885805899455,22.6146358479788,46.));
#22069=CARTESIAN_POINT('Ctrl Pts',(54.1137702212827,21.7689600531191,46.));
#22070=CARTESIAN_POINT('Ctrl Pts',(53.267851387655,20.6527649215947,46.0000000000001));
#22071=CARTESIAN_POINT('Ctrl Pts',(52.6132688313215,19.9575001862921,45.9999999999999));
#22072=CARTESIAN_POINT('Ctrl Pts',(52.0600422917726,19.6355082498452,46.0000000000001));
#22073=CARTESIAN_POINT('Ctrl Pts',(51.7092971610549,19.5959179422654,46.));
#22074=CARTESIAN_POINT('Ctrl Pts',(54.8498454495129,22.8208715049056,45.1947514602968));
#22075=CARTESIAN_POINT('Ctrl Pts',(54.4276728878709,22.4046326878925,45.2688266414859));
#22076=CARTESIAN_POINT('Ctrl Pts',(53.7584764072867,21.670812023264,45.4340456995033));
#22077=CARTESIAN_POINT('Ctrl Pts',(52.9162294593297,20.6402827270753,45.7053535607057));
#22078=CARTESIAN_POINT('Ctrl Pts',(52.3583769742476,19.9751884160731,45.8895956767591));
#22079=CARTESIAN_POINT('Ctrl Pts',(51.9502746726906,19.6521457104047,45.9816693098607));
#22080=CARTESIAN_POINT('Ctrl Pts',(51.7092971610549,19.5959179422654,46.));
#22081=CARTESIAN_POINT('Ctrl Pts',(54.1372439325421,22.9065587328174,44.4304270626387));
#22082=CARTESIAN_POINT('Ctrl Pts',(53.7472447505792,22.4964832086346,44.6462611267445));
#22083=CARTESIAN_POINT('Ctrl Pts',(53.1541646175812,21.7560680203378,45.0210196472744));
#22084=CARTESIAN_POINT('Ctrl Pts',(52.4850075211232,20.6995709152847,45.5168050506341));
#22085=CARTESIAN_POINT('Ctrl Pts',(52.0911343848321,20.0136370147741,45.8210758339952));
#22086=CARTESIAN_POINT('Ctrl Pts',(51.840758511164,19.6707821067247,45.968114937896));
#22087=CARTESIAN_POINT('Ctrl Pts',(51.7092971610549,19.5959179422654,46.));
#22088=CARTESIAN_POINT('Ctrl Pts',(53.3864876668068,23.3160685609229,44.2307692320894));
#22089=CARTESIAN_POINT('Ctrl Pts',(53.0439951189989,22.8358340303902,44.4839588612342));
#22090=CARTESIAN_POINT('Ctrl Pts',(52.5423502486883,21.9908524941898,44.9125177602508));
#22091=CARTESIAN_POINT('Ctrl Pts',(52.0530341102106,20.8197959816443,45.4633470605684));
#22092=CARTESIAN_POINT('Ctrl Pts',(51.8239020992648,20.0709136872745,45.7962695577249));
#22093=CARTESIAN_POINT('Ctrl Pts',(51.7312389779497,19.6914330268016,45.959302575355));
#22094=CARTESIAN_POINT('Ctrl Pts',(51.7092971610549,19.5959179422654,46.));
#22095=CARTESIAN_POINT('Origin',(53.3864876668068,24.2487113033598,46.000000001373));
#22096=CARTESIAN_POINT('Ctrl Pts',(55.035992162965,23.1177228342965,46.));
#22097=CARTESIAN_POINT('Ctrl Pts',(54.3299192064178,22.0879417672428,46.));
#22098=CARTESIAN_POINT('Ctrl Pts',(53.8230715593574,21.3650115665077,46.));
#22099=CARTESIAN_POINT('Ctrl Pts',(53.0821556643503,20.4538645006679,46.));
#22100=CARTESIAN_POINT('Ctrl Pts',(52.7982587176799,20.151721721479,46.));
#22101=CARTESIAN_POINT('Ctrl Pts',(52.3967587125637,19.8400027811804,46.));
#22102=CARTESIAN_POINT('Ctrl Pts',(52.2554329542124,19.7480371194989,46.0000000000325));
#22103=CARTESIAN_POINT('Ctrl Pts',(52.0414383936788,19.6565556786848,46.0000000000325));
#22104=CARTESIAN_POINT('Ctrl Pts',(51.9738964717323,19.6337322451885,46.));
#22105=CARTESIAN_POINT('Ctrl Pts',(51.8404098310991,19.6038714213037,46.));
#22106=CARTESIAN_POINT('Ctrl Pts',(51.7751374400014,19.5959179422654,46.));
#22107=CARTESIAN_POINT('Ctrl Pts',(51.7092971610549,19.5959179422654,46.));
#22108=CARTESIAN_POINT('Ctrl Pts',(69.9640078370513,23.1177228342728,46.));
#22109=CARTESIAN_POINT('Ctrl Pts',(69.542232429734,23.7328665315065,46.));
#22110=CARTESIAN_POINT('Ctrl Pts',(68.5372497203374,24.8762781693712,46.));
#22111=CARTESIAN_POINT('Ctrl Pts',(66.5003162911619,26.2518765973163,46.));
#22112=CARTESIAN_POINT('Ctrl Pts',(63.9229202346607,27.0854099302792,46.));
#22113=CARTESIAN_POINT('Ctrl Pts',(61.0682561393548,27.0809097910938,46.));
#22114=CARTESIAN_POINT('Ctrl Pts',(58.4978723140799,26.2506120287296,46.));
#22115=CARTESIAN_POINT('Ctrl Pts',(56.4626291503929,24.8770023535894,46.));
#22116=CARTESIAN_POINT('Ctrl Pts',(55.4536863537726,23.7269142298698,46.));
#22117=CARTESIAN_POINT('Ctrl Pts',(55.0359921615024,23.1177228321634,46.));
#22118=CARTESIAN_POINT('Ctrl Pts',(70.0200075221065,23.036049382692,45.7722265692886));
#22119=CARTESIAN_POINT('Ctrl Pts',(69.5701845212888,23.6267219749651,45.7450333341526));
#22120=CARTESIAN_POINT('Ctrl Pts',(68.5033702547963,24.6932485864254,45.7248984528665));
#22121=CARTESIAN_POINT('Ctrl Pts',(66.4423862476702,25.9202843643973,45.7851490895574));
#22122=CARTESIAN_POINT('Ctrl Pts',(63.9082001948719,26.6583896707281,45.8854558492519));
#22123=CARTESIAN_POINT('Ctrl Pts',(61.0833863606388,26.6544061954588,45.8839043324688));
#22124=CARTESIAN_POINT('Ctrl Pts',(58.5556906298045,25.9185765932678,45.7844483918357));
#22125=CARTESIAN_POINT('Ctrl Pts',(56.4966824739014,24.6938781056256,45.7240522007472));
#22126=CARTESIAN_POINT('Ctrl Pts',(55.4254628658836,23.6210064625855,45.7452964634328));
#22127=CARTESIAN_POINT('Ctrl Pts',(54.9799924763511,23.0360493806665,45.772226569382));
#22128=CARTESIAN_POINT('Ctrl Pts',(70.2092197650832,22.9256684193351,45.3167264994702));
#22129=CARTESIAN_POINT('Ctrl Pts',(69.7158291105167,23.4853279772436,45.2164752999052));
#22130=CARTESIAN_POINT('Ctrl Pts',(68.535014472362,24.4361203670811,45.0981257954975));
#22131=CARTESIAN_POINT('Ctrl Pts',(66.383710902278,25.3846466842565,45.1588861842134));
#22132=CARTESIAN_POINT('Ctrl Pts',(63.8865686721771,25.8842035797987,45.3602142350906));
#22133=CARTESIAN_POINT('Ctrl Pts',(61.1051010280161,25.8825087356241,45.3567819163901));
#22134=CARTESIAN_POINT('Ctrl Pts',(58.6143395050501,25.3831984355184,45.1570202136384));
#22135=CARTESIAN_POINT('Ctrl Pts',(56.4652796759868,24.4374218336232,45.0958734343921));
#22136=CARTESIAN_POINT('Ctrl Pts',(55.279396703872,23.479912555679,45.2174453583462));
#22137=CARTESIAN_POINT('Ctrl Pts',(54.7907802332251,22.9256684174159,45.316726499814));
#22138=CARTESIAN_POINT('Ctrl Pts',(70.6459692050112,22.9403123749432,44.776430516514));
#22139=CARTESIAN_POINT('Ctrl Pts',(70.1274758860988,23.5168125343884,44.5569401518289));
#22140=CARTESIAN_POINT('Ctrl Pts',(68.8339836677725,24.4521830465394,44.2171354911649));
#22141=CARTESIAN_POINT('Ctrl Pts',(66.4852650826246,25.2255541487752,44.0484187526542));
#22142=CARTESIAN_POINT('Ctrl Pts',(63.8933590415983,25.4907416731797,44.1400917531453));
#22143=CARTESIAN_POINT('Ctrl Pts',(61.0969988006743,25.4920128625193,44.1369164712371));
#22144=CARTESIAN_POINT('Ctrl Pts',(58.5131163976547,25.2255225866375,44.0466798604088));
#22145=CARTESIAN_POINT('Ctrl Pts',(56.1663207696582,24.4550752730798,44.2144948710689));
#22146=CARTESIAN_POINT('Ctrl Pts',(54.8675070278469,23.5112341585235,44.5590640016228));
#22147=CARTESIAN_POINT('Ctrl Pts',(54.3540307932109,22.9403123729663,44.7764305172667));
#22148=CARTESIAN_POINT('Ctrl Pts',(71.13576024646,23.0841835154325,44.412288853233));
#22149=CARTESIAN_POINT('Ctrl Pts',(70.6147355135831,23.7210088220381,44.0947795647742));
#22150=CARTESIAN_POINT('Ctrl Pts',(69.2492273035993,24.7560226484019,43.5531210449959));
#22151=CARTESIAN_POINT('Ctrl Pts',(66.6913084652411,25.5729841387648,43.1242832122387));
#22152=CARTESIAN_POINT('Ctrl Pts',(63.9257521800277,25.7932760987112,43.0406381319293));
#22153=CARTESIAN_POINT('Ctrl Pts',(61.0627975487631,25.7956751380647,43.0388168513456));
#22154=CARTESIAN_POINT('Ctrl Pts',(58.3074986944687,25.5736178460725,43.1233746593592));
#22155=CARTESIAN_POINT('Ctrl Pts',(55.7509094065862,24.7598092206675,43.5507965518109));
#22156=CARTESIAN_POINT('Ctrl Pts',(54.3802229056199,23.7148467232691,44.0978518729798));
#22157=CARTESIAN_POINT('Ctrl Pts',(53.8642397517534,23.0841835132488,44.4122888543217));
#22158=CARTESIAN_POINT('Ctrl Pts',(71.4542425639415,23.2306116904396,44.2758174708167));
#22159=CARTESIAN_POINT('Ctrl Pts',(70.9372237337292,23.9223005711455,43.9129480259072));
#22160=CARTESIAN_POINT('Ctrl Pts',(69.5371396621711,25.0636258970674,43.2733988845769));
#22161=CARTESIAN_POINT('Ctrl Pts',(66.8466481816036,25.991977143232,42.7149637246248));
#22162=CARTESIAN_POINT('Ctrl Pts',(63.9528070871081,26.2647811407212,42.546738631874));
#22163=CARTESIAN_POINT('Ctrl Pts',(61.0345041648995,26.2670739944513,42.5455363906498));
#22164=CARTESIAN_POINT('Ctrl Pts',(58.1524504628798,25.9925148535544,42.714387867757));
#22165=CARTESIAN_POINT('Ctrl Pts',(55.4628430152718,25.0675639103996,43.2712020277055));
#22166=CARTESIAN_POINT('Ctrl Pts',(54.0577734476554,23.9156075971566,43.9164592516275));
#22167=CARTESIAN_POINT('Ctrl Pts',(53.5457574342856,23.2306116880677,44.275817472061));
#22168=CARTESIAN_POINT('Ctrl Pts',(71.6135123314272,23.3160685633993,44.2307692307839));
#22169=CARTESIAN_POINT('Ctrl Pts',(71.0985268893462,24.038267655457,43.8500649418989));
#22170=CARTESIAN_POINT('Ctrl Pts',(69.681226557465,25.239555364586,43.1717497595138));
#22171=CARTESIAN_POINT('Ctrl Pts',(66.9244886027247,26.2356604580669,42.5652091566662));
#22172=CARTESIAN_POINT('Ctrl Pts',(63.9663874943631,26.5460492373018,42.3707472230138));
#22173=CARTESIAN_POINT('Ctrl Pts',(61.020309894555,26.5481066493621,42.3696710366589));
#22174=CARTESIAN_POINT('Ctrl Pts',(58.0747486677894,26.2360703120526,42.564673612103));
#22175=CARTESIAN_POINT('Ctrl Pts',(55.3186828044349,25.2435158958716,43.1695330127632));
#22176=CARTESIAN_POINT('Ctrl Pts',(53.8964899676441,24.0312794561666,43.8537487425402));
#22177=CARTESIAN_POINT('Ctrl Pts',(53.3864876668068,23.3160685609229,44.2307692320894));
#22178=CARTESIAN_POINT('Origin',(71.6135123314049,24.2487113059679,45.9999999999981));
#22179=CARTESIAN_POINT('Ctrl Pts',(73.2907035679191,19.5959179422654,46.));
#22180=CARTESIAN_POINT('Ctrl Pts',(73.2853132736892,19.5959179422654,46.));
#22181=CARTESIAN_POINT('Ctrl Pts',(73.2800921964744,19.5959613316258,46.));
#22182=CARTESIAN_POINT('Ctrl Pts',(73.190737153897,19.5979267180889,46.));
#22183=CARTESIAN_POINT('Ctrl Pts',(73.0919541682948,19.6164825507722,46.));
#22184=CARTESIAN_POINT('Ctrl Pts',(72.9349512659537,19.6613683597688,46.));
#22185=CARTESIAN_POINT('Ctrl Pts',(72.7366254879835,19.7544322191794,46.));
#22186=CARTESIAN_POINT('Ctrl Pts',(72.5187524776661,19.8974562011792,46.));
#22187=CARTESIAN_POINT('Ctrl Pts',(72.3059356178939,20.0751969944156,46.));
#22188=CARTESIAN_POINT('Ctrl Pts',(72.1177575559123,20.2549369737277,46.));
#22189=CARTESIAN_POINT('Ctrl Pts',(71.9467703806141,20.4356656328949,46.));
#22190=CARTESIAN_POINT('Ctrl Pts',(71.7871832912953,20.6165764559116,46.));
#22191=CARTESIAN_POINT('Ctrl Pts',(71.6363028797942,20.7973306481917,46.));
#22192=CARTESIAN_POINT('Ctrl Pts',(71.4916909653841,20.977997589463,46.));
#22193=CARTESIAN_POINT('Ctrl Pts',(71.3520460598813,21.1584331287946,46.));
#22194=CARTESIAN_POINT('Ctrl Pts',(71.2162849549212,21.3385618577325,46.));
#22195=CARTESIAN_POINT('Ctrl Pts',(71.1057852053627,21.488374549024,46.));
#22196=CARTESIAN_POINT('Ctrl Pts',(71.0186156532208,21.6080221976867,46.));
#22197=CARTESIAN_POINT('Ctrl Pts',(70.8890085638933,21.7872920165661,46.));
#22198=CARTESIAN_POINT('Ctrl Pts',(70.7410429419584,21.9958939832604,46.));
#22199=CARTESIAN_POINT('Ctrl Pts',(70.5744311075321,22.2333786866411,46.));
#22200=CARTESIAN_POINT('Ctrl Pts',(70.409440490942,22.4703098380079,46.));
#22201=CARTESIAN_POINT('Ctrl Pts',(70.2056431651792,22.765428405125,46.));
#22202=CARTESIAN_POINT('Ctrl Pts',(70.0444070209061,23.0004636239141,46.));
#22203=CARTESIAN_POINT('Ctrl Pts',(69.9640078370348,23.1177228342968,46.));
#22204=CARTESIAN_POINT('Ctrl Pts',(73.2907035679191,19.5959179422654,46.));
#22205=CARTESIAN_POINT('Ctrl Pts',(73.2862490793568,19.5960900665757,45.9999175533143));
#22206=CARTESIAN_POINT('Ctrl Pts',(73.2820811790803,19.5963336271153,45.9998440681509));
#22207=CARTESIAN_POINT('Ctrl Pts',(73.208253200484,19.6010450092914,45.9982213945468));
#22208=CARTESIAN_POINT('Ctrl Pts',(73.1274794573141,19.6220399195827,45.9943050481736));
#22209=CARTESIAN_POINT('Ctrl Pts',(72.9963653350095,19.6695017870272,45.9858046677887));
#22210=CARTESIAN_POINT('Ctrl Pts',(72.8294716734784,19.764069356512,45.9701218125784));
#22211=CARTESIAN_POINT('Ctrl Pts',(72.6414650292326,19.9063529120636,45.9471817238329));
#22212=CARTESIAN_POINT('Ctrl Pts',(72.4536342973198,20.081311370936,45.9196661796449));
#22213=CARTESIAN_POINT('Ctrl Pts',(72.2835895740479,20.2570788809575,45.8924066669206));
#22214=CARTESIAN_POINT('Ctrl Pts',(72.1258636290523,20.4329402115168,45.8655395060906));
#22215=CARTESIAN_POINT('Ctrl Pts',(71.9757248574748,20.6082090575464,45.8391421338054));
#22216=CARTESIAN_POINT('Ctrl Pts',(71.8311830958701,20.7826098635032,45.8132826543535));
#22217=CARTESIAN_POINT('Ctrl Pts',(71.6902708461682,20.9562249829189,45.7879723330246));
#22218=CARTESIAN_POINT('Ctrl Pts',(71.5520244073844,21.1289170402946,45.7632628720577));
#22219=CARTESIAN_POINT('Ctrl Pts',(71.4156157450574,21.3006067154702,45.7392000949141));
#22220=CARTESIAN_POINT('Ctrl Pts',(71.3030395865729,21.4428000487426,45.7197248605149));
#22221=CARTESIAN_POINT('Ctrl Pts',(71.2133703207735,21.5559942629584,45.7045133261289));
#22222=CARTESIAN_POINT('Ctrl Pts',(71.0792059015168,21.7252227168858,45.6820761723759));
#22223=CARTESIAN_POINT('Ctrl Pts',(70.9236830208857,21.9210467851455,45.6570406101074));
#22224=CARTESIAN_POINT('Ctrl Pts',(70.7457968935764,22.1424153277308,45.630177451962));
#22225=CARTESIAN_POINT('Ctrl Pts',(70.5678883520528,22.3622036711249,45.6045437380644));
#22226=CARTESIAN_POINT('Ctrl Pts',(70.3450747297217,22.6339353529314,45.5749261951409));
#22227=CARTESIAN_POINT('Ctrl Pts',(70.165943219464,22.8481046901869,45.5540871152153));
#22228=CARTESIAN_POINT('Ctrl Pts',(70.0760072071431,22.9543759311333,45.5444531385751));
#22229=CARTESIAN_POINT('Ctrl Pts',(73.2907035679191,19.5959179422654,46.));
#22230=CARTESIAN_POINT('Ctrl Pts',(73.2880504840915,19.5964289578032,45.9997781423769));
#22231=CARTESIAN_POINT('Ctrl Pts',(73.2853846053994,19.5969457764203,45.9995692096135));
#22232=CARTESIAN_POINT('Ctrl Pts',(73.2411647337054,19.6070786822663,45.995310811962));
#22233=CARTESIAN_POINT('Ctrl Pts',(73.1895361350525,19.6323355913422,45.9857343837773));
#22234=CARTESIAN_POINT('Ctrl Pts',(73.1063585625323,19.6861977169776,45.96540896875));
#22235=CARTESIAN_POINT('Ctrl Pts',(72.9951136441404,19.7861798679065,45.9282889331739));
#22236=CARTESIAN_POINT('Ctrl Pts',(72.8650301145033,19.9324850330593,45.8739794495604));
#22237=CARTESIAN_POINT('Ctrl Pts',(72.7278523001271,20.1091863830438,45.8082212986075));
#22238=CARTESIAN_POINT('Ctrl Pts',(72.599008386305,20.2853439277712,45.7422966248579));
#22239=CARTESIAN_POINT('Ctrl Pts',(72.4749524884831,20.4604229392962,45.6764333722182));
#22240=CARTESIAN_POINT('Ctrl Pts',(72.3531838593419,20.634045289074,45.6107610623116));
#22241=CARTESIAN_POINT('Ctrl Pts',(72.2325138280896,20.8059659224486,45.545403805715));
#22242=CARTESIAN_POINT('Ctrl Pts',(72.1118213239367,20.9763160140027,45.4803379945738));
#22243=CARTESIAN_POINT('Ctrl Pts',(71.9905611813765,21.1449425524697,45.4156563653195));
#22244=CARTESIAN_POINT('Ctrl Pts',(71.8682925794356,21.3117528991958,45.3514312058611));
#22245=CARTESIAN_POINT('Ctrl Pts',(71.7653253439371,21.4491702215447,45.2983550050255));
#22246=CARTESIAN_POINT('Ctrl Pts',(71.682174619526,21.5581056496617,45.2561979636126));
#22247=CARTESIAN_POINT('Ctrl Pts',(71.5566443241353,21.7204926694612,45.1932855292725));
#22248=CARTESIAN_POINT('Ctrl Pts',(71.4078049567651,21.9069447194497,45.1208830261352));
#22249=CARTESIAN_POINT('Ctrl Pts',(71.2337951661038,22.1155847374877,45.0398130889285));
#22250=CARTESIAN_POINT('Ctrl Pts',(71.0572027402818,22.3211899834939,44.9599661565235));
#22251=CARTESIAN_POINT('Ctrl Pts',(70.8314760697034,22.5723353005728,44.8626519726254));
#22252=CARTESIAN_POINT('Ctrl Pts',(70.6454769955238,22.7666605685381,44.787912840376));
#22253=CARTESIAN_POINT('Ctrl Pts',(70.5510931890894,22.8620875206656,44.7514416370933));
#22254=CARTESIAN_POINT('Ctrl Pts',(73.2907035679191,19.5959179422654,46.));
#22255=CARTESIAN_POINT('Ctrl Pts',(73.2897792520886,19.5967541971494,45.9996437628225));
#22256=CARTESIAN_POINT('Ctrl Pts',(73.288766733936,19.5975749243332,45.9992940960059));
#22257=CARTESIAN_POINT('Ctrl Pts',(73.2730749026927,19.6130270044881,45.9927106906892));
#22258=CARTESIAN_POINT('Ctrl Pts',(73.251756086113,19.6437149190236,45.9796188466631));
#22259=CARTESIAN_POINT('Ctrl Pts',(73.216079179159,19.7062122776897,45.9528815794702));
#22260=CARTESIAN_POINT('Ctrl Pts',(73.1625244070959,19.8168600337209,45.9053443493137));
#22261=CARTESIAN_POINT('Ctrl Pts',(73.0934344901874,19.975480126619,45.8366125412608));
#22262=CARTESIAN_POINT('Ctrl Pts',(73.0131490016378,20.1651666288159,45.7534836745954));
#22263=CARTESIAN_POINT('Ctrl Pts',(72.9327871582964,20.3538190600323,45.6698774417649));
#22264=CARTESIAN_POINT('Ctrl Pts',(72.8511054586688,20.5411597726202,45.5859293751855));
#22265=CARTESIAN_POINT('Ctrl Pts',(72.7674694094519,20.7270595237571,45.5017127400763));
#22266=CARTESIAN_POINT('Ctrl Pts',(72.6815224957815,20.9113376828887,45.417327487362));
#22267=CARTESIAN_POINT('Ctrl Pts',(72.5928892631333,21.0942091320849,45.3326926851353));
#22268=CARTESIAN_POINT('Ctrl Pts',(72.5014236904482,21.2755404995838,45.24788633318));
#22269=CARTESIAN_POINT('Ctrl Pts',(72.4070183371161,21.4552564835779,45.1629622322214));
#22270=CARTESIAN_POINT('Ctrl Pts',(72.3258429327874,21.603596996729,45.0921463541392));
#22271=CARTESIAN_POINT('Ctrl Pts',(72.2593780519087,21.7213758855668,45.0354955830711));
#22272=CARTESIAN_POINT('Ctrl Pts',(72.1581530560203,21.8971298392077,44.9505368909156));
#22273=CARTESIAN_POINT('Ctrl Pts',(72.0355742524663,22.0994507797852,44.8515128507767));
#22274=CARTESIAN_POINT('Ctrl Pts',(71.8893300919241,22.3266244145461,44.7387188968997));
#22275=CARTESIAN_POINT('Ctrl Pts',(71.7390041704018,22.5509982091827,44.6262592382376));
#22276=CARTESIAN_POINT('Ctrl Pts',(71.5434859051336,22.8260292236067,44.4864687330478));
#22277=CARTESIAN_POINT('Ctrl Pts',(71.3791052619253,23.0398714682527,44.3758130784414));
#22278=CARTESIAN_POINT('Ctrl Pts',(71.2949727964356,23.1451548175056,44.320865710836));
#22279=CARTESIAN_POINT('Ctrl Pts',(73.2907035679191,19.5959179422654,46.));
#22280=CARTESIAN_POINT('Ctrl Pts',(73.2904808728319,19.5968857094338,45.9995877329126));
#22281=CARTESIAN_POINT('Ctrl Pts',(73.2902587582729,19.5978534806893,45.9991754285667));
#22282=CARTESIAN_POINT('Ctrl Pts',(73.2862090342068,19.6154867193585,45.9916623858903));
#22283=CARTESIAN_POINT('Ctrl Pts',(73.278471643703,19.6487953456216,45.977449084781));
#22284=CARTESIAN_POINT('Ctrl Pts',(73.2626675329748,19.7153221034526,45.9489756536103));
#22285=CARTESIAN_POINT('Ctrl Pts',(73.2341485984696,19.8314987172849,45.8990281581236));
#22286=CARTESIAN_POINT('Ctrl Pts',(73.1909498335265,19.9967609507555,45.8273396719058));
#22287=CARTESIAN_POINT('Ctrl Pts',(73.1352131070871,20.1938738237251,45.7408225076835));
#22288=CARTESIAN_POINT('Ctrl Pts',(73.0755852718533,20.3897951762557,45.6538223879631));
#22289=CARTESIAN_POINT('Ctrl Pts',(73.0121109467716,20.5844107113345,45.5664035981079));
#22290=CARTESIAN_POINT('Ctrl Pts',(72.9448178995343,20.7776647362872,45.4786056970811));
#22291=CARTESIAN_POINT('Ctrl Pts',(72.8737703412485,20.969415619956,45.3905097941917));
#22292=CARTESIAN_POINT('Ctrl Pts',(72.7988814082159,21.1599111909158,45.302017540834));
#22293=CARTESIAN_POINT('Ctrl Pts',(72.7201916785671,21.3490306679124,45.2131989345674));
#22294=CARTESIAN_POINT('Ctrl Pts',(72.6377280503905,21.5367060266982,45.1241021330032));
#22295=CARTESIAN_POINT('Ctrl Pts',(72.5658930280084,21.6918256295662,45.0496717620424));
#22296=CARTESIAN_POINT('Ctrl Pts',(72.5065732598677,21.8151167092688,44.990045399374));
#22297=CARTESIAN_POINT('Ctrl Pts',(72.4157517404387,21.9992281010938,44.9005387053819));
#22298=CARTESIAN_POINT('Ctrl Pts',(72.3044475744177,22.211560601306,44.7959596617311));
#22299=CARTESIAN_POINT('Ctrl Pts',(72.1700773346563,22.4505358369901,44.6764670164254));
#22300=CARTESIAN_POINT('Ctrl Pts',(72.0309897669014,22.6869514584429,44.557072726346));
#22301=CARTESIAN_POINT('Ctrl Pts',(71.8483990288815,22.9774859633438,44.4081667977607));
#22302=CARTESIAN_POINT('Ctrl Pts',(71.6932714543115,23.2042169236777,44.2897313638428));
#22303=CARTESIAN_POINT('Ctrl Pts',(71.6135123314072,23.3160685634275,44.2307692307691));
#22304=CARTESIAN_POINT('Ctrl Pts',(73.2907028389451,19.5959179422654,46.));
#22305=CARTESIAN_POINT('Ctrl Pts',(73.1782488824317,19.5959179422654,46.));
#22306=CARTESIAN_POINT('Ctrl Pts',(73.0679692680469,19.6191095759631,46.0000000000001));
#22307=CARTESIAN_POINT('Ctrl Pts',(72.7990151985813,19.7161705537826,46.0000000000001));
#22308=CARTESIAN_POINT('Ctrl Pts',(72.6442834670101,19.8115682299362,45.999999999991));
#22309=CARTESIAN_POINT('Ctrl Pts',(72.2391188325035,20.1170685085798,45.999999999991));
#22310=CARTESIAN_POINT('Ctrl Pts',(71.9632856619516,20.4043146233181,46.));
#22311=CARTESIAN_POINT('Ctrl Pts',(71.2192192201258,21.3045670772791,46.));
#22312=CARTESIAN_POINT('Ctrl Pts',(70.6968197820516,22.0489439500589,46.));
#22313=CARTESIAN_POINT('Ctrl Pts',(69.964007837035,23.1177228342965,46.));
#22314=CARTESIAN_POINT('Ctrl Pts',(55.035992162965,23.1177228342965,46.));
#22315=CARTESIAN_POINT('Ctrl Pts',(54.0296627127653,21.6500288723272,46.9446698131654));
#22316=CARTESIAN_POINT('Ctrl Pts',(52.8893156673895,18.1414957976349,48.915242890626));
#22317=CARTESIAN_POINT('Ctrl Pts',(54.5395958207989,12.4855237992675,50.8957649600243));
#22318=CARTESIAN_POINT('Ctrl Pts',(59.4315484638286,8.79278472652513,51.5632592674646));
#22319=CARTESIAN_POINT('Ctrl Pts',(65.5663223673701,8.80057359018861,51.5646626464224));
#22320=CARTESIAN_POINT('Ctrl Pts',(70.463129301692,12.4814952571317,50.8974409168532));
#22321=CARTESIAN_POINT('Ctrl Pts',(72.1120278968484,18.1410701930242,48.9161444008817));
#22322=CARTESIAN_POINT('Ctrl Pts',(70.9703446072329,21.6500181963829,46.944676684654));
#22323=CARTESIAN_POINT('Ctrl Pts',(69.964007837035,23.1177228342965,46.));
#22324=CARTESIAN_POINT('Ctrl Pts',(54.9799924779109,23.0360493827148,45.7722265692876));
#22325=CARTESIAN_POINT('Ctrl Pts',(53.9836364614215,21.5483875117231,46.7011217010093));
#22326=CARTESIAN_POINT('Ctrl Pts',(52.8947746067151,18.0181392478017,48.6325382140834));
#22327=CARTESIAN_POINT('Ctrl Pts',(54.5878793708661,12.4419398028121,50.5700934772302));
#22328=CARTESIAN_POINT('Ctrl Pts',(59.4430893598328,8.79596203843427,51.238449475546));
#22329=CARTESIAN_POINT('Ctrl Pts',(65.55434777324,8.80321749148772,51.2397703452684));
#22330=CARTESIAN_POINT('Ctrl Pts',(70.41476928952,12.438794404978,50.5716603603405));
#22331=CARTESIAN_POINT('Ctrl Pts',(72.1066202548239,18.0180329314669,48.6333855335872));
#22332=CARTESIAN_POINT('Ctrl Pts',(71.0163707860304,21.5483766905331,46.7011284577535));
#22333=CARTESIAN_POINT('Ctrl Pts',(70.0200075220891,23.0360493827148,45.7722265692876));
#22334=CARTESIAN_POINT('Ctrl Pts',(54.7907372267642,22.9258570992293,45.3170284863951));
#22335=CARTESIAN_POINT('Ctrl Pts',(53.7919468056835,21.3912213348628,46.2144683518221));
#22336=CARTESIAN_POINT('Ctrl Pts',(52.7562467146473,17.7832971764642,48.0679863059215));
#22337=CARTESIAN_POINT('Ctrl Pts',(54.5366561274746,12.2550558273829,49.9200347179853));
#22338=CARTESIAN_POINT('Ctrl Pts',(59.4130828744335,8.63727200384955,50.5900930650603));
#22339=CARTESIAN_POINT('Ctrl Pts',(65.5836888418126,8.64389537621032,50.5912639994337));
#22340=CARTESIAN_POINT('Ctrl Pts',(70.4660116067358,12.2531404542804,49.9213697367866));
#22341=CARTESIAN_POINT('Ctrl Pts',(72.2451937624934,17.7836520803225,48.0687233931725));
#22342=CARTESIAN_POINT('Ctrl Pts',(71.2080604594761,21.3912101719866,46.2144748797621));
#22343=CARTESIAN_POINT('Ctrl Pts',(70.2092627732358,22.9258570992293,45.3170284863951));
#22344=CARTESIAN_POINT('Ctrl Pts',(54.2349613371585,22.9441110925392,44.6287642460336));
#22345=CARTESIAN_POINT('Ctrl Pts',(53.1616750836308,21.3176435330343,45.4948761270818));
#22346=CARTESIAN_POINT('Ctrl Pts',(52.0452054104636,17.4934953607748,47.2745378463438));
#22347=CARTESIAN_POINT('Ctrl Pts',(53.9548569140681,11.6579928841,49.0503090096131));
#22348=CARTESIAN_POINT('Ctrl Pts',(59.1876493330094,7.84833229000289,49.7160755075247));
#22349=CARTESIAN_POINT('Ctrl Pts',(65.8088963456918,7.85518686750345,49.7170728023697));
#22350=CARTESIAN_POINT('Ctrl Pts',(71.0479870198883,11.6561154937289,49.0515269255847));
#22351=CARTESIAN_POINT('Ctrl Pts',(72.9563437045815,17.4939164999665,47.2752004277968));
#22352=CARTESIAN_POINT('Ctrl Pts',(71.8383327234084,21.3176317021775,45.4948824271433));
#22353=CARTESIAN_POINT('Ctrl Pts',(70.7650386628414,22.9441110925392,44.6287642460336));
#22354=CARTESIAN_POINT('Ctrl Pts',(53.7050272035642,23.1451548175054,44.3208657108362));
#22355=CARTESIAN_POINT('Ctrl Pts',(52.5348398293169,21.4555874814272,45.2026346040126));
#22356=CARTESIAN_POINT('Ctrl Pts',(51.2465470842867,17.4440228922175,47.0300555365631));
#22357=CARTESIAN_POINT('Ctrl Pts',(53.2226320825593,11.1174259777979,48.8622205971348));
#22358=CARTESIAN_POINT('Ctrl Pts',(58.9168123145029,6.9913313904512,49.5150230715549));
#22359=CARTESIAN_POINT('Ctrl Pts',(66.0802655944533,6.9993885995003,49.5163292093625));
#22360=CARTESIAN_POINT('Ctrl Pts',(71.7804277049591,11.1138898217104,48.8634707307727));
#22361=CARTESIAN_POINT('Ctrl Pts',(73.7550958709857,17.4439130956519,47.0307891232465));
#22362=CARTESIAN_POINT('Ctrl Pts',(72.4651686825769,21.4555751915853,45.2026410179626));
#22363=CARTESIAN_POINT('Ctrl Pts',(71.2949727964358,23.1451548175054,44.3208657108362));
#22364=CARTESIAN_POINT('Ctrl Pts',(53.3864876685926,23.3160685634272,44.2307692307692));
#22365=CARTESIAN_POINT('Ctrl Pts',(52.1577649697301,21.5929471992367,45.1391055895821));
#22366=CARTESIAN_POINT('Ctrl Pts',(50.7654075275861,17.4738130645841,47.0338873948327));
#22367=CARTESIAN_POINT('Ctrl Pts',(52.780390477329,10.8335144477163,48.9382355384849));
#22368=CARTESIAN_POINT('Ctrl Pts',(58.7534376271057,6.49811636507681,49.5800569879468));
#22369=CARTESIAN_POINT('Ctrl Pts',(66.2439626695514,6.50726074921208,49.5814063907908));
#22370=CARTESIAN_POINT('Ctrl Pts',(72.2229368821765,10.828784805706,48.9398470354358));
#22371=CARTESIAN_POINT('Ctrl Pts',(74.2362329569254,17.4733133906627,47.034754231617));
#22372=CARTESIAN_POINT('Ctrl Pts',(72.8422439679473,21.5929346653242,45.1391121967827));
#22373=CARTESIAN_POINT('Ctrl Pts',(71.6135123314074,23.3160685634272,44.2307692307692));
#22374=CARTESIAN_POINT('Ctrl Pts',(69.9640078388351,23.1177228316711,-46.));
#22375=CARTESIAN_POINT('Ctrl Pts',(70.4282880935365,22.448394502084,-46.0000000000001));
#22376=CARTESIAN_POINT('Ctrl Pts',(71.1098490068872,21.4276043550564,-46.));
#22377=CARTESIAN_POINT('Ctrl Pts',(72.1079771651491,20.2176388416739,-46.));
#22378=CARTESIAN_POINT('Ctrl Pts',(72.7378313921175,19.7052440604699,-46.));
#22379=CARTESIAN_POINT('Ctrl Pts',(73.2907028389451,19.5959179422654,-46.));
#22380=CARTESIAN_POINT('Ctrl Pts',(70.150154550487,22.8208715049056,-45.1947514602968));
#22381=CARTESIAN_POINT('Ctrl Pts',(70.7132801788335,22.2671987041132,-45.2933824298082));
#22382=CARTESIAN_POINT('Ctrl Pts',(71.4994124151429,21.3677327932072,-45.5083661587332));
#22383=CARTESIAN_POINT('Ctrl Pts',(72.4178953923351,20.2269070318774,-45.8190912488055));
#22384=CARTESIAN_POINT('Ctrl Pts',(72.9072401408116,19.7267421723513,-45.9597943306481));
#22385=CARTESIAN_POINT('Ctrl Pts',(73.2907028389451,19.5959179422654,-46.));
#22386=CARTESIAN_POINT('Ctrl Pts',(70.862756067458,22.9065587328173,-44.4304270626387));
#22387=CARTESIAN_POINT('Ctrl Pts',(71.3824929671134,22.3609404106397,-44.7176762130643));
#22388=CARTESIAN_POINT('Ctrl Pts',(72.0706374133237,21.4474353285422,-45.1743630927634));
#22389=CARTESIAN_POINT('Ctrl Pts',(72.7587045416073,20.2739035226561,-45.7078285895115));
#22390=CARTESIAN_POINT('Ctrl Pts',(73.0771229289095,19.7538948849925,-45.9327798968234));
#22391=CARTESIAN_POINT('Ctrl Pts',(73.2907028389451,19.5959179422654,-46.));
#22392=CARTESIAN_POINT('Ctrl Pts',(71.6135123331932,23.3160685609229,-44.2307692320894));
#22393=CARTESIAN_POINT('Ctrl Pts',(72.0694661900611,22.6771055141269,-44.5677393482618));
#22394=CARTESIAN_POINT('Ctrl Pts',(72.6451832973973,21.6425621324406,-45.085801261871));
#22395=CARTESIAN_POINT('Ctrl Pts',(73.099528966838,20.3540492246571,-45.6728025929409));
#22396=CARTESIAN_POINT('Ctrl Pts',(73.2470092805887,19.7866035098537,-45.918783509084));
#22397=CARTESIAN_POINT('Ctrl Pts',(73.2907028389451,19.5959179422654,-46.));
#22398=CARTESIAN_POINT('',(69.9640078388351,23.1177228316711,-46.0000000008449));
#22399=CARTESIAN_POINT('Origin',(71.6135123331932,24.2487113033598,-46.000000001373));
#22400=CARTESIAN_POINT('Ctrl Pts',(69.964007837035,23.1177228342965,-46.));
#22401=CARTESIAN_POINT('Ctrl Pts',(70.6700807935817,22.0879417672436,-46.));
#22402=CARTESIAN_POINT('Ctrl Pts',(71.1769284406424,21.365011566508,-46.));
#22403=CARTESIAN_POINT('Ctrl Pts',(71.9178443356484,20.4538645006696,-46.));
#22404=CARTESIAN_POINT('Ctrl Pts',(72.2017412823191,20.1517217214797,-46.));
#22405=CARTESIAN_POINT('Ctrl Pts',(72.6032412874365,19.8400027811803,-46.));
#22406=CARTESIAN_POINT('Ctrl Pts',(72.7445670457876,19.748037119499,-46.0000000000325));
#22407=CARTESIAN_POINT('Ctrl Pts',(72.958561606321,19.656555678685,-46.0000000000325));
#22408=CARTESIAN_POINT('Ctrl Pts',(73.0261035282676,19.6337322451886,-46.));
#22409=CARTESIAN_POINT('Ctrl Pts',(73.1595901689006,19.6038714213038,-46.));
#22410=CARTESIAN_POINT('Ctrl Pts',(73.2248625599985,19.5959179422654,-46.));
#22411=CARTESIAN_POINT('Ctrl Pts',(73.2907028389451,19.5959179422654,-46.));
#22412=CARTESIAN_POINT('Ctrl Pts',(55.0359921629487,23.1177228342728,-46.));
#22413=CARTESIAN_POINT('Ctrl Pts',(55.4577675702659,23.7328665315063,-46.));
#22414=CARTESIAN_POINT('Ctrl Pts',(56.4644460987129,24.8770406742655,-46.));
#22415=CARTESIAN_POINT('Ctrl Pts',(58.4968877073687,26.2505571664569,-46.));
#22416=CARTESIAN_POINT('Ctrl Pts',(61.0767126915491,27.0852062473976,-46.));
#22417=CARTESIAN_POINT('Ctrl Pts',(63.9310735094902,27.0805880901559,-46.));
#22418=CARTESIAN_POINT('Ctrl Pts',(66.5019245727494,26.2505063992629,-46.));
#22419=CARTESIAN_POINT('Ctrl Pts',(68.5371826391601,24.876911244511,-46.));
#22420=CARTESIAN_POINT('Ctrl Pts',(69.5463136462273,23.72691422987,-46.));
#22421=CARTESIAN_POINT('Ctrl Pts',(69.9640078384976,23.1177228321634,-46.));
#22422=CARTESIAN_POINT('Ctrl Pts',(54.9799924778935,23.036049382692,-45.7722265692886));
#22423=CARTESIAN_POINT('Ctrl Pts',(55.429815478711,23.6267219749649,-45.7450333341526));
#22424=CARTESIAN_POINT('Ctrl Pts',(56.4988342870035,24.6938856008765,-45.7247629982864));
#22425=CARTESIAN_POINT('Ctrl Pts',(58.5542027836181,25.9190899660437,-45.7850931685235));
#22426=CARTESIAN_POINT('Ctrl Pts',(61.0913426462871,26.65821922096,-45.8854831073846));
#22427=CARTESIAN_POINT('Ctrl Pts',(63.9157961167037,26.6541165160517,-45.8838942577118));
#22428=CARTESIAN_POINT('Ctrl Pts',(66.4440587647699,25.9184853590342,-45.7844551748528));
#22429=CARTESIAN_POINT('Ctrl Pts',(68.5030877198132,24.6937964378016,-45.7240503148626));
#22430=CARTESIAN_POINT('Ctrl Pts',(69.5745371341163,23.6210064625856,-45.7452964634328));
#22431=CARTESIAN_POINT('Ctrl Pts',(70.0200075236488,23.0360493806665,-45.772226569382));
#22432=CARTESIAN_POINT('Ctrl Pts',(54.7907802349192,22.9256684193329,-45.3167264994694));
#22433=CARTESIAN_POINT('Ctrl Pts',(55.2841708894856,23.4853279772414,-45.2164752999044));
#22434=CARTESIAN_POINT('Ctrl Pts',(56.4679989024545,24.4367980894975,-45.0977591258001));
#22435=CARTESIAN_POINT('Ctrl Pts',(58.6119105347406,25.3836007202491,-45.1590251424147));
#22436=CARTESIAN_POINT('Ctrl Pts',(61.112821395526,25.8840372741794,-45.3603121455667));
#22437=CARTESIAN_POINT('Ctrl Pts',(63.8938482330649,25.8822538891794,-45.3568243041171));
#22438=CARTESIAN_POINT('Ctrl Pts',(66.3853316497856,25.3831132440572,-45.1570554139588));
#22439=CARTESIAN_POINT('Ctrl Pts',(68.5344243155597,24.4373495148053,-45.0958874813595));
#22440=CARTESIAN_POINT('Ctrl Pts',(69.7206032961255,23.479912555677,-45.2174453583454));
#22441=CARTESIAN_POINT('Ctrl Pts',(70.2092197667725,22.9256684174138,-45.3167264998131));
#22442=CARTESIAN_POINT('Ctrl Pts',(54.3540307949898,22.940312374942,-44.7764305165133));
#22443=CARTESIAN_POINT('Ctrl Pts',(54.8725241139022,23.5168125343872,-44.5569401518282));
#22444=CARTESIAN_POINT('Ctrl Pts',(56.1694841702895,24.4531474854901,-44.2164314277651));
#22445=CARTESIAN_POINT('Ctrl Pts',(58.5098618481284,25.2243797451509,-44.0490074515783));
#22446=CARTESIAN_POINT('Ctrl Pts',(61.1059304240575,25.4905041608905,-44.1402636454315));
#22447=CARTESIAN_POINT('Ctrl Pts',(63.901828202477,25.4917212441726,-44.1370682351324));
#22448=CARTESIAN_POINT('Ctrl Pts',(66.4865076249529,25.2254109591687,-44.0467524245259));
#22449=CARTESIAN_POINT('Ctrl Pts',(68.8333479287006,24.4549911624279,-44.2145400319697));
#22450=CARTESIAN_POINT('Ctrl Pts',(70.132492972152,23.5112341585224,-44.5590640016221));
#22451=CARTESIAN_POINT('Ctrl Pts',(70.6459692067881,22.9403123729652,-44.776430517266));
#22452=CARTESIAN_POINT('Ctrl Pts',(53.8642397535411,23.0841835154313,-44.4122888532322));
#22453=CARTESIAN_POINT('Ctrl Pts',(54.3852644864179,23.7210088220369,-44.0947795647735));
#22454=CARTESIAN_POINT('Ctrl Pts',(55.7542433739063,24.7573036807876,-43.5521310136212));
#22455=CARTESIAN_POINT('Ctrl Pts',(58.3038539355888,25.5714931127472,-43.1253852425921));
#22456=CARTESIAN_POINT('Ctrl Pts',(61.0735166591671,25.7929641498958,-43.0408658934962));
#22457=CARTESIAN_POINT('Ctrl Pts',(63.9360342309663,25.7953039701295,-43.0390901749241));
#22458=CARTESIAN_POINT('Ctrl Pts',(66.692119856051,25.5734728698309,-43.1234808632927));
#22459=CARTESIAN_POINT('Ctrl Pts',(69.2487599668007,24.7597018881128,-43.5508755354234));
#22460=CARTESIAN_POINT('Ctrl Pts',(70.619777094379,23.714846723268,-44.097851872979));
#22461=CARTESIAN_POINT('Ctrl Pts',(71.1357602482455,23.0841835132476,-44.4122888543209));
#22462=CARTESIAN_POINT('Ctrl Pts',(53.5457574360584,23.2306116904395,-44.2758174708167));
#22463=CARTESIAN_POINT('Ctrl Pts',(54.0627762662708,23.9223005711454,-43.9129480259072));
#22464=CARTESIAN_POINT('Ctrl Pts',(55.4662284705153,25.0651176112046,-43.2722290901921));
#22465=CARTESIAN_POINT('Ctrl Pts',(58.1486595615419,25.9902484809716,-42.7163490041473));
#22466=CARTESIAN_POINT('Ctrl Pts',(61.0464675813894,26.2644288113384,-42.547000973267));
#22467=CARTESIAN_POINT('Ctrl Pts',(63.9643601544157,26.2666452488003,-42.5458771037084));
#22468=CARTESIAN_POINT('Ctrl Pts',(66.847174393407,25.9923497630692,-42.7145138052446));
#22469=CARTESIAN_POINT('Ctrl Pts',(69.5368351511896,25.0674401569483,-43.2712998655934));
#22470=CARTESIAN_POINT('Ctrl Pts',(70.9422265523446,23.9156075971566,-43.9164592516275));
#22471=CARTESIAN_POINT('Ctrl Pts',(71.4542425657144,23.2306116880677,-44.2758174720609));
#22472=CARTESIAN_POINT('Ctrl Pts',(53.3864876685727,23.3160685633993,-44.2307692307839));
#22473=CARTESIAN_POINT('Ctrl Pts',(53.9014731106537,24.038267655457,-43.8500649418989));
#22474=CARTESIAN_POINT('Ctrl Pts',(55.3220849100951,25.2411372376895,-43.1704876695772));
#22475=CARTESIAN_POINT('Ctrl Pts',(58.0708968314258,26.2337622543912,-42.5667104493236));
#22476=CARTESIAN_POINT('Ctrl Pts',(61.0328912216257,26.5456758334602,-42.3710278989254));
#22477=CARTESIAN_POINT('Ctrl Pts',(63.9785719433368,26.5476372801886,-42.3700397756168));
#22478=CARTESIAN_POINT('Ctrl Pts',(66.9248798545188,26.2358932678842,-42.5648089417427));
#22479=CARTESIAN_POINT('Ctrl Pts',(69.681000122088,25.243380770632,-43.1696388054261));
#22480=CARTESIAN_POINT('Ctrl Pts',(71.1035100323559,24.0312794561666,-43.8537487425401));
#22481=CARTESIAN_POINT('Ctrl Pts',(71.6135123331932,23.3160685609229,-44.2307692320894));
#22482=CARTESIAN_POINT('',(55.0359921629504,23.1177228342752,-46.0000000000069));
#22483=CARTESIAN_POINT('Origin',(53.3864876685947,24.2487113059674,-45.9999999999984));
#22484=CARTESIAN_POINT('Origin',(62.5,18.,-46.));
#22485=CARTESIAN_POINT('Ctrl Pts',(51.7092971610549,19.5959179422654,-46.));
#22486=CARTESIAN_POINT('Ctrl Pts',(52.2620653939839,19.7051356050392,-46.));
#22487=CARTESIAN_POINT('Ctrl Pts',(52.8920949226161,20.2177543439005,-46.));
#22488=CARTESIAN_POINT('Ctrl Pts',(53.8897778317011,21.4271096929168,-45.9999999999999));
#22489=CARTESIAN_POINT('Ctrl Pts',(54.5713813881105,22.4479061064219,-46.0000000000001));
#22490=CARTESIAN_POINT('Ctrl Pts',(55.0359921629652,23.1177228342968,-46.));
#22491=CARTESIAN_POINT('Ctrl Pts',(51.7092971610548,19.5959179422654,-46.));
#22492=CARTESIAN_POINT('Ctrl Pts',(52.0926675666913,19.7266394067263,-45.9598226817129));
#22493=CARTESIAN_POINT('Ctrl Pts',(52.5821841468467,20.2270134514137,-45.819062250804));
#22494=CARTESIAN_POINT('Ctrl Pts',(53.5002246591862,21.3672689127023,-45.5084940953287));
#22495=CARTESIAN_POINT('Ctrl Pts',(54.2863195908853,22.2667867790925,-45.2934650574444));
#22496=CARTESIAN_POINT('Ctrl Pts',(54.849845451707,22.8208715070777,-45.194751459911));
#22497=CARTESIAN_POINT('Ctrl Pts',(51.709297161055,19.5959179422654,-46.));
#22498=CARTESIAN_POINT('Ctrl Pts',(51.9228095515637,19.753788288119,-45.9328286977184));
#22499=CARTESIAN_POINT('Ctrl Pts',(52.2413619039012,20.2740130336108,-45.7077763242479));
#22500=CARTESIAN_POINT('Ctrl Pts',(52.9290812390771,21.4469571597183,-45.1745842010763));
#22501=CARTESIAN_POINT('Ctrl Pts',(53.6171415340253,22.3605295352944,-44.7178900299161));
#22502=CARTESIAN_POINT('Ctrl Pts',(54.1372439345722,22.9065587349562,-44.4304270615132));
#22503=CARTESIAN_POINT('Ctrl Pts',(51.7092971610549,19.5959179422654,-46.));
#22504=CARTESIAN_POINT('Ctrl Pts',(51.7529482282219,19.7864858334401,-45.9188374584652));
#22505=CARTESIAN_POINT('Ctrl Pts',(51.9005239862315,20.3541704296053,-45.6727447106325));
#22506=CARTESIAN_POINT('Ctrl Pts',(52.3546179283007,21.6420362564594,-45.0860447448006));
#22507=CARTESIAN_POINT('Ctrl Pts',(52.930215177034,22.6766294615115,-44.5679874350866));
#22508=CARTESIAN_POINT('Ctrl Pts',(53.3864876685928,23.3160685634274,-44.2307692307691));
#22509=CARTESIAN_POINT('Ctrl Pts',(51.7092971610549,19.5959179422654,-46.));
#22510=CARTESIAN_POINT('Ctrl Pts',(52.2620653939839,19.7051356050392,-46.));
#22511=CARTESIAN_POINT('Ctrl Pts',(52.4720752368613,19.876008517993,-46.));
#22512=CARTESIAN_POINT('Ctrl Pts',(52.659590508736,20.0475121432486,-46.));
#22513=CARTESIAN_POINT('Ctrl Pts',(53.0346210524853,20.39051939376,-46.));
#22514=CARTESIAN_POINT('Ctrl Pts',(53.3196733122239,20.7360494934789,-46.));
#22515=CARTESIAN_POINT('Ctrl Pts',(53.5854418805396,21.0798247170144,-46.));
#22516=CARTESIAN_POINT('Ctrl Pts',(54.1169790171708,21.7673751640851,-46.));
#22517=CARTESIAN_POINT('Ctrl Pts',(54.5713813881103,22.4479061064217,-46.0000000000001));
#22518=CARTESIAN_POINT('Ctrl Pts',(55.035992162965,23.1177228342965,-46.));
#22519=CARTESIAN_POINT('Ctrl Pts',(69.964007837035,23.1177228342965,-46.));
#22520=CARTESIAN_POINT('Ctrl Pts',(70.9703372872347,21.6500288723272,-46.9446698131655));
#22521=CARTESIAN_POINT('Ctrl Pts',(72.1183944604502,18.1446538308373,-48.9200122557279));
#22522=CARTESIAN_POINT('Ctrl Pts',(70.4543334202127,12.483202392177,-50.8920744141013));
#22523=CARTESIAN_POINT('Ctrl Pts',(65.5691776348049,8.79342862675378,-51.5637399768993));
#22524=CARTESIAN_POINT('Ctrl Pts',(59.4328684025022,8.80019559553396,-51.5641637407931));
#22525=CARTESIAN_POINT('Ctrl Pts',(54.5371355691,12.4816854912179,-50.8976114017526));
#22526=CARTESIAN_POINT('Ctrl Pts',(52.8878093794935,18.1409814039487,-48.9160426988189));
#22527=CARTESIAN_POINT('Ctrl Pts',(54.0296553927672,21.650018196383,-46.944676684654));
#22528=CARTESIAN_POINT('Ctrl Pts',(55.035992162965,23.1177228342965,-46.));
#22529=CARTESIAN_POINT('Ctrl Pts',(70.0200075220892,23.0360493827148,-45.7722265692876));
#22530=CARTESIAN_POINT('Ctrl Pts',(71.0163635385786,21.548387511723,-46.7011217010093));
#22531=CARTESIAN_POINT('Ctrl Pts',(72.1116609454533,18.0207073641069,-48.6369541642022));
#22532=CARTESIAN_POINT('Ctrl Pts',(70.4070372012184,12.4400174548645,-50.5666834109832));
#22533=CARTESIAN_POINT('Ctrl Pts',(65.5574758632647,8.79647831783238,-51.238894394837));
#22534=CARTESIAN_POINT('Ctrl Pts',(59.444982641667,8.80290739556665,-51.2393092746466));
#22535=CARTESIAN_POINT('Ctrl Pts',(54.5854421071155,12.438947874978,-50.5718180574722));
#22536=CARTESIAN_POINT('Ctrl Pts',(52.8932465944024,18.0179605889219,-48.6332915172475));
#22537=CARTESIAN_POINT('Ctrl Pts',(53.9836292139696,21.5483766905331,-46.7011284577535));
#22538=CARTESIAN_POINT('Ctrl Pts',(54.9799924779108,23.0360493827148,-45.7722265692876));
#22539=CARTESIAN_POINT('Ctrl Pts',(70.2092627732358,22.9258570992293,-45.3170284863951));
#22540=CARTESIAN_POINT('Ctrl Pts',(71.2080531943165,21.3912213348628,-46.2144683518222));
#22541=CARTESIAN_POINT('Ctrl Pts',(72.2485073332692,17.7848938426267,-48.0716979134992));
#22542=CARTESIAN_POINT('Ctrl Pts',(70.4595522749644,12.2538636517655,-49.9171964156177));
#22543=CARTESIAN_POINT('Ctrl Pts',(65.5872688285877,8.63757133840816,-50.5904626682655));
#22544=CARTESIAN_POINT('Ctrl Pts',(59.4158247717921,8.64370707313489,-50.5908806139701));
#22545=CARTESIAN_POINT('Ctrl Pts',(54.5341291044486,12.2532305473249,-49.9215007698885));
#22546=CARTESIAN_POINT('Ctrl Pts',(52.7547119853049,17.7836087469459,-48.0686452362413));
#22547=CARTESIAN_POINT('Ctrl Pts',(53.7919395405239,21.3912101719867,-46.2144748797621));
#22548=CARTESIAN_POINT('Ctrl Pts',(54.7907372267642,22.9258570992293,-45.3170284863951));
#22549=CARTESIAN_POINT('Ctrl Pts',(70.7650386628415,22.9441110925393,-44.6287642460337));
#22550=CARTESIAN_POINT('Ctrl Pts',(71.8383249163693,21.3176435330343,-45.4948761270819));
#22551=CARTESIAN_POINT('Ctrl Pts',(72.9598945847606,17.4948749234169,-47.277728446391));
#22552=CARTESIAN_POINT('Ctrl Pts',(71.0410755502145,11.6569613647031,-49.047848196163));
#22553=CARTESIAN_POINT('Ctrl Pts',(65.8127297003932,7.84860393154229,-49.7164030171663));
#22554=CARTESIAN_POINT('Ctrl Pts',(59.1905815389834,7.85502151184498,-49.7167388747517));
#22555=CARTESIAN_POINT('Ctrl Pts',(53.9521643544241,11.6561965293243,-49.0516422890679));
#22556=CARTESIAN_POINT('Ctrl Pts',(52.0435550568373,17.4938780779608,-47.2751321156197));
#22557=CARTESIAN_POINT('Ctrl Pts',(53.1616672765916,21.3176317021776,-45.4948824271434));
#22558=CARTESIAN_POINT('Ctrl Pts',(54.2349613371585,22.9441110925393,-44.6287642460337));
#22559=CARTESIAN_POINT('Ctrl Pts',(71.2949727964358,23.1451548175053,-44.3208657108362));
#22560=CARTESIAN_POINT('Ctrl Pts',(72.4651601706831,21.4555874814272,-45.2026346040127));
#22561=CARTESIAN_POINT('Ctrl Pts',(73.7611756319396,17.4466520281733,-47.0338832915689));
#22562=CARTESIAN_POINT('Ctrl Pts',(71.7712823336433,11.1154328342175,-48.8593967521573));
#22563=CARTESIAN_POINT('Ctrl Pts',(66.0838726210504,6.99188921257162,-49.5153685816591));
#22564=CARTESIAN_POINT('Ctrl Pts',(58.9189313583151,6.99906255642572,-49.5159529203514));
#22565=CARTESIAN_POINT('Ctrl Pts',(53.2198273601607,11.1140544776842,-48.8635955038756));
#22566=CARTESIAN_POINT('Ctrl Pts',(51.24474414428,17.443836399062,-47.0307131526209));
#22567=CARTESIAN_POINT('Ctrl Pts',(52.5348313174231,21.4555751915854,-45.2026410179625));
#22568=CARTESIAN_POINT('Ctrl Pts',(53.7050272035642,23.1451548175053,-44.3208657108362));
#22569=CARTESIAN_POINT('Ctrl Pts',(71.6135123314074,23.3160685634272,-44.2307692307692));
#22570=CARTESIAN_POINT('Ctrl Pts',(72.84223503027,21.5929471992366,-45.1391055895822));
#22571=CARTESIAN_POINT('Ctrl Pts',(74.2440064959087,17.4775207002499,-47.0384733228152));
#22572=CARTESIAN_POINT('Ctrl Pts',(72.2121971594862,10.8307890388393,-48.9346869366359));
#22573=CARTESIAN_POINT('Ctrl Pts',(66.2474489353142,6.49887232528998,-49.580519208557));
#22574=CARTESIAN_POINT('Ctrl Pts',(58.7550492649336,6.50681697095731,-49.5809266738395));
#22575=CARTESIAN_POINT('Ctrl Pts',(52.7773865235972,10.8290081468293,-48.9400109632237));
#22576=CARTESIAN_POINT('Ctrl Pts',(50.7635683583871,17.4732091493448,-47.0346564411719));
#22577=CARTESIAN_POINT('Ctrl Pts',(52.1577560320527,21.5929346653243,-45.1391121967827));
#22578=CARTESIAN_POINT('Ctrl Pts',(53.3864876685926,23.3160685634272,-44.2307692307692));
#22579=CARTESIAN_POINT('',(53.4480382353792,18.0006404973954,-48.7869877464486));
#22580=CARTESIAN_POINT('Ctrl Pts',(69.9640078386373,23.1177228319597,-46.0000000015041));
#22581=CARTESIAN_POINT('Ctrl Pts',(70.970337287844,21.6500288704668,-46.9446698142138));
#22582=CARTESIAN_POINT('Ctrl Pts',(72.1183944601558,18.1446538298357,-48.9200122560767));
#22583=CARTESIAN_POINT('Ctrl Pts',(70.4543334202127,12.483202392177,-50.8920744141013));
#22584=CARTESIAN_POINT('Ctrl Pts',(65.5691776348049,8.79342862675378,-51.5637399768993));
#22585=CARTESIAN_POINT('Ctrl Pts',(59.4328684025022,8.80019559553396,-51.5641637407931));
#22586=CARTESIAN_POINT('Ctrl Pts',(54.5593513886519,12.4649796541169,-50.9006360779329));
#22587=CARTESIAN_POINT('Ctrl Pts',(53.4526536488011,16.20324910153,-49.5945088774883));
#22588=CARTESIAN_POINT('Ctrl Pts',(53.4480382353792,18.0006404973954,-48.7869877464486));
#22589=CARTESIAN_POINT('Ctrl Pts',(53.4480382353792,18.0006404973954,-48.7869877464486));
#22590=CARTESIAN_POINT('Ctrl Pts',(53.4479745368625,18.025446761822,-48.7758429380598));
#22591=CARTESIAN_POINT('Ctrl Pts',(53.450960195781,19.8716148791025,-47.9437781664976));
#22592=CARTESIAN_POINT('Ctrl Pts',(54.0296553927672,21.650018196383,-46.944676684654));
#22593=CARTESIAN_POINT('Ctrl Pts',(55.035992162965,23.1177228342965,-46.));
#22594=CARTESIAN_POINT('Origin',(62.5,18.,-64.));
#22595=CARTESIAN_POINT('',(53.45,18.,-64.));
#22596=CARTESIAN_POINT('Origin',(99.8,45.,-45.));
#22597=CARTESIAN_POINT('Origin',(99.8,-45.,45.));
#22598=CARTESIAN_POINT('Origin',(99.8,45.,45.));
#22599=CARTESIAN_POINT('Origin',(99.8,-45.,-45.));
#22600=CARTESIAN_POINT('Origin',(-4.8,0.,0.));
#22601=CARTESIAN_POINT('',(-9.5,-23.525,-2.88098159499415E-15));
#22602=CARTESIAN_POINT('Origin',(-9.5,0.,0.));
#22603=CARTESIAN_POINT('',(0.,-23.525,-2.88098159499415E-15));
#22604=CARTESIAN_POINT('',(-4.8,-23.525,-2.88098159499415E-15));
#22605=CARTESIAN_POINT('Origin',(0.,0.,0.));
#22606=CARTESIAN_POINT('Origin',(0.,27.505,0.));
#22607=CARTESIAN_POINT('',(-1.11022302462516E-15,-27.505,-3.36839102105479E-15));
#22608=CARTESIAN_POINT('Origin',(0.,0.,0.));
#22609=CARTESIAN_POINT('Origin',(6.99999999999999,0.,0.));
#22610=CARTESIAN_POINT('',(14.,-27.505,-3.36839102105479E-15));
#22611=CARTESIAN_POINT('',(6.99999999999999,-27.505,-3.36839102105479E-15));
#22612=CARTESIAN_POINT('Origin',(14.,0.,0.));
#22613=CARTESIAN_POINT('Origin',(14.,26.,0.));
#22614=CARTESIAN_POINT('',(14.,-26.,-3.18408167778312E-15));
#22615=CARTESIAN_POINT('Origin',(14.,0.,0.));
#22616=CARTESIAN_POINT('Origin',(15.,0.,0.));
#22617=CARTESIAN_POINT('',(16.,-26.,-3.18408167778312E-15));
#22618=CARTESIAN_POINT('',(15.,-26.,-3.18408167778312E-15));
#22619=CARTESIAN_POINT('Origin',(16.,0.,0.));
#22620=CARTESIAN_POINT('Origin',(16.,50.,0.));
#22621=CARTESIAN_POINT('Origin',(-9.5,50.3,0.));
#22622=CARTESIAN_POINT('Origin',(16.,-32.,32.));
#22623=CARTESIAN_POINT('Origin',(16.,-32.,-32.));
#22624=CARTESIAN_POINT('Origin',(16.,0.,0.));
#22625=CARTESIAN_POINT('Origin',(16.,0.,0.));
#22626=CARTESIAN_POINT('',(0.,0.,0.));
#22627=CARTESIAN_POINT('Origin',(151.05,0.,0.));
#22628=CARTESIAN_POINT('',(150.8,13.5,-1.65327317884893E-15));
#22629=CARTESIAN_POINT('Origin',(150.8,0.,0.));
#22630=CARTESIAN_POINT('',(151.3,13.,1.59204083889156E-15));
#22631=CARTESIAN_POINT('',(151.05,13.25,-1.62265700887024E-15));
#22632=CARTESIAN_POINT('',(151.3,-13.,-1.59204083889156E-15));
#22633=CARTESIAN_POINT('Origin',(151.3,0.,0.));
#22634=CARTESIAN_POINT('Origin',(151.3,0.,0.));
#22635=CARTESIAN_POINT('Origin',(150.8,13.,0.));
#22636=CARTESIAN_POINT('',(150.8,-16.505,-2.02127954199271E-15));
#22637=CARTESIAN_POINT('Origin',(150.8,0.,0.));
#22638=CARTESIAN_POINT('Origin',(152.8,0.,0.));
#22639=CARTESIAN_POINT('',(154.8,-13.,-1.59204083889156E-15));
#22640=CARTESIAN_POINT('',(152.8,-13.,-1.59204083889156E-15));
#22641=CARTESIAN_POINT('Origin',(154.8,0.,0.));
#22642=CARTESIAN_POINT('Origin',(150.,-79.75,0.));
#22643=CARTESIAN_POINT('',(130.5,-80.,-2.38806125833734E-15));
#22644=CARTESIAN_POINT('Origin',(150.,-80.,0.));
#22645=CARTESIAN_POINT('',(131.,-79.5,2.32682891837997E-15));
#22646=CARTESIAN_POINT('',(130.75,-79.75,-2.35744508835865E-15));
#22647=CARTESIAN_POINT('Origin',(150.,-79.5,0.));
#22648=CARTESIAN_POINT('Origin',(125.8,-80.,-42.));
#22649=CARTESIAN_POINT('',(163.678669277077,-80.,40.));
#22650=CARTESIAN_POINT('',(173.,-80.,30.9027787310304));
#22651=CARTESIAN_POINT('Origin',(167.85,-80.,34.95));
#22652=CARTESIAN_POINT('',(136.321330722923,-80.,40.));
#22653=CARTESIAN_POINT('',(138.1,-80.,40.));
#22654=CARTESIAN_POINT('',(127.8,-80.,30.0530621813219));
#22655=CARTESIAN_POINT('Origin',(132.15,-80.,34.95));
#22656=CARTESIAN_POINT('',(127.8,-80.,-30.0530621813219));
#22657=CARTESIAN_POINT('',(127.8,-80.,-21.));
#22658=CARTESIAN_POINT('',(136.321330722923,-80.,-40.));
#22659=CARTESIAN_POINT('Origin',(132.15,-80.,-34.95));
#22660=CARTESIAN_POINT('',(163.678669277077,-80.,-40.));
#22661=CARTESIAN_POINT('',(138.1,-80.,-40.));
#22662=CARTESIAN_POINT('',(173.,-80.,-30.9027787310304));
#22663=CARTESIAN_POINT('Origin',(167.85,-80.,-34.95));
#22664=CARTESIAN_POINT('',(173.,-80.,-21.));
#22665=CARTESIAN_POINT('Origin',(150.,-80.,0.));
#22666=CARTESIAN_POINT('',(131.0005787145,-35.9988802797138,0.000387228748759416));
#22667=CARTESIAN_POINT('',(131.,-80.,2.32682891837997E-15));
#22668=CARTESIAN_POINT('',(131.,-20.,2.32682891837997E-15));
#22669=CARTESIAN_POINT('Ctrl Pts',(131.,-20.,3.7470027081099E-15));
#22670=CARTESIAN_POINT('Ctrl Pts',(131.,-20.,0.861580403347818));
#22671=CARTESIAN_POINT('Ctrl Pts',(131.062882219654,-20.177547250434,1.72325967716755));
#22672=CARTESIAN_POINT('Ctrl Pts',(131.166407061299,-20.4957587354358,2.50630832645151));
#22673=CARTESIAN_POINT('Ctrl Pts',(131.269931902945,-20.8139702204376,3.28935697573546));
#22674=CARTESIAN_POINT('Ctrl Pts',(131.414099366581,-21.2728459400074,3.99377500048364));
#22675=CARTESIAN_POINT('Ctrl Pts',(131.566890134667,-21.8297157892228,4.60514959406471));
#22676=CARTESIAN_POINT('Ctrl Pts',(131.719680902753,-22.3865856384382,5.21652418764578));
#22677=CARTESIAN_POINT('Ctrl Pts',(131.881094975289,-23.0414496172992,5.73485535005976));
#22678=CARTESIAN_POINT('Ctrl Pts',(132.022932148162,-23.7812715599426,6.14978270902572));
#22679=CARTESIAN_POINT('Ctrl Pts',(132.164769321036,-24.521093502586,6.5647100679917));
#22680=CARTESIAN_POINT('Ctrl Pts',(132.287029594247,-25.3458734090118,6.87623362350966));
#22681=CARTESIAN_POINT('Ctrl Pts',(132.359109453404,-26.218038076651,7.05638957039791));
#22682=CARTESIAN_POINT('Ctrl Pts',(132.407162692842,-26.7994811884105,7.17649353499007));
#22683=CARTESIAN_POINT('Ctrl Pts',(132.432913526034,-27.4019841940426,7.23821189574679));
#22684=CARTESIAN_POINT('Ctrl Pts',(132.432837348447,-28.0029670680466,7.23818290361787));
#22685=CARTESIAN_POINT('Ctrl Pts',(132.432761170859,-28.6039499420506,7.23815391148896));
#22686=CARTESIAN_POINT('Ctrl Pts',(132.406857982492,-29.2034126844264,7.17637756647439));
#22687=CARTESIAN_POINT('Ctrl Pts',(132.358699643159,-29.7840623655322,7.05586397232987));
#22688=CARTESIAN_POINT('Ctrl Pts',(132.310541303825,-30.3647120466379,6.93535037818535));
#22689=CARTESIAN_POINT('Ctrl Pts',(132.240127813526,-30.9265486664736,6.75609953491087));
#22690=CARTESIAN_POINT('Ctrl Pts',(132.156532403699,-31.4546224725911,6.52774573987559));
#22691=CARTESIAN_POINT('Ctrl Pts',(131.989341584043,-32.5107700848262,6.07103814980503));
#22692=CARTESIAN_POINT('Ctrl Pts',(131.769423086272,-33.4318664421888,5.41791875269127));
#22693=CARTESIAN_POINT('Ctrl Pts',(131.5661054454,-34.1731638593317,4.60441612118007));
#22694=CARTESIAN_POINT('Ctrl Pts',(131.464446624964,-34.5438125679032,4.19766480542447));
#22695=CARTESIAN_POINT('Ctrl Pts',(131.366938018753,-34.8695115414198,3.75081768106951));
#22696=CARTESIAN_POINT('Ctrl Pts',(131.282292361583,-35.1407839851041,3.2643108477403));
#22697=CARTESIAN_POINT('Ctrl Pts',(131.155323875828,-35.5476926506305,2.5345505977465));
#22698=CARTESIAN_POINT('Ctrl Pts',(131.057297025417,-35.8321416240344,1.71555600256064));
#22699=CARTESIAN_POINT('Ctrl Pts',(131.019156861914,-35.9439288801667,0.861916886569704));
#22700=CARTESIAN_POINT('Ctrl Pts',(131.006445419458,-35.9811855970535,0.577414055312998));
#22701=CARTESIAN_POINT('Ctrl Pts',(131.000386017092,-35.9992635494311,0.289063010818519));
#22702=CARTESIAN_POINT('Ctrl Pts',(131.000681403705,-35.9986815924753,0.000455940025769347));
#22703=CARTESIAN_POINT('Origin',(150.,-20.,0.));
#22704=CARTESIAN_POINT('',(132.432701479047,-28.,-7.23809523809524));
#22705=CARTESIAN_POINT('Ctrl Pts',(132.432701479047,-28.,-7.23809523809524));
#22706=CARTESIAN_POINT('Ctrl Pts',(132.432701479047,-26.8009816752416,-7.23809523809524));
#22707=CARTESIAN_POINT('Ctrl Pts',(132.321869554036,-25.6008229172718,-6.98274855048125));
#22708=CARTESIAN_POINT('Ctrl Pts',(132.155628452105,-24.545670137385,-6.52703527428346));
#22709=CARTESIAN_POINT('Ctrl Pts',(132.07250790114,-24.0180937474416,-6.29917863618456));
#22710=CARTESIAN_POINT('Ctrl Pts',(131.975535055945,-23.5267688520189,-6.02123035093972));
#22711=CARTESIAN_POINT('Ctrl Pts',(131.874197516921,-23.0724682732237,-5.69922103670885));
#22712=CARTESIAN_POINT('Ctrl Pts',(131.671522438873,-22.1638671156332,-5.05520240824711));
#22713=CARTESIAN_POINT('Ctrl Pts',(131.451388585508,-21.4033632245524,-4.23493966384127));
#22714=CARTESIAN_POINT('Ctrl Pts',(131.282228165024,-20.8608983376114,-3.26382017119042));
#22715=CARTESIAN_POINT('Ctrl Pts',(131.197647954782,-20.5896658941409,-2.778260424865));
#22716=CARTESIAN_POINT('Ctrl Pts',(131.12581110276,-20.3729432017053,-2.25498649147832));
#22717=CARTESIAN_POINT('Ctrl Pts',(131.076399114064,-20.22552672817,-1.7039165396102));
#22718=CARTESIAN_POINT('Ctrl Pts',(131.026987125369,-20.0781102546348,-1.15284658774209));
#22719=CARTESIAN_POINT('Ctrl Pts',(131.,-20.,-0.573980617392535));
#22720=CARTESIAN_POINT('Ctrl Pts',(131.,-20.,3.88578058618805E-15));
#22721=CARTESIAN_POINT('Ctrl Pts',(131.000681403705,-35.9986815924753,0.000455940025769347));
#22722=CARTESIAN_POINT('Ctrl Pts',(131.001272312551,-35.9975174113732,-0.57689070813748));
#22723=CARTESIAN_POINT('Ctrl Pts',(131.027294049206,-35.9216793201183,-1.15526193173957));
#22724=CARTESIAN_POINT('Ctrl Pts',(131.076366966692,-35.7753210194057,-1.70590043958833));
#22725=CARTESIAN_POINT('Ctrl Pts',(131.14997071157,-35.5558003636517,-2.53179501295942));
#22726=CARTESIAN_POINT('Ctrl Pts',(131.27543167792,-35.1776335132831,-3.29530052290559));
#22727=CARTESIAN_POINT('Ctrl Pts',(131.418812458471,-34.6912990154186,-3.96691479885595));
#22728=CARTESIAN_POINT('Ctrl Pts',(131.562193239021,-34.2049645175541,-4.63852907480631));
#22729=CARTESIAN_POINT('Ctrl Pts',(131.723493833771,-33.6104623721938,-5.21825211676085));
#22730=CARTESIAN_POINT('Ctrl Pts',(131.875295509315,-32.9286711143801,-5.70073440851176));
#22731=CARTESIAN_POINT('Ctrl Pts',(132.027097184859,-32.2468798565664,-6.18321670026267));
#22732=CARTESIAN_POINT('Ctrl Pts',(132.169399941196,-31.4777994862994,-6.56845824180994));
#22733=CARTESIAN_POINT('Ctrl Pts',(132.270801014743,-30.6410546041911,-6.83217787626808));
#22734=CARTESIAN_POINT('Ctrl Pts',(132.37220208829,-29.8043097220827,-7.09589751072622));
#22735=CARTESIAN_POINT('Ctrl Pts',(132.432701479047,-28.899900328133,-7.23809523809524));
#22736=CARTESIAN_POINT('Ctrl Pts',(132.432701479047,-28.,-7.23809523809524));
#22737=CARTESIAN_POINT('Origin',(167.85,-79.75,34.95));
#22738=CARTESIAN_POINT('',(172.606870229008,-79.5,31.2117269195014));
#22739=CARTESIAN_POINT('',(173.,-80.,30.9027787310304));
#22740=CARTESIAN_POINT('',(161.8,-79.5,34.95));
#22741=CARTESIAN_POINT('Origin',(167.85,-79.5,34.95));
#22742=CARTESIAN_POINT('',(163.997091469667,-79.5,39.6145038167939));
#22743=CARTESIAN_POINT('Origin',(167.85,-79.5,34.95));
#22744=CARTESIAN_POINT('',(163.997091469667,-79.5,39.6145038167939));
#22745=CARTESIAN_POINT('Ctrl Pts',(164.24404266268,-79.9563089001744,40.4157589290663));
#22746=CARTESIAN_POINT('Ctrl Pts',(164.904763645791,-79.8656939616692,40.8421377709704));
#22747=CARTESIAN_POINT('Ctrl Pts',(165.655411043149,-79.6645622818713,41.125231372512));
#22748=CARTESIAN_POINT('Ctrl Pts',(166.910806630347,-79.4726177418242,41.3575474685077));
#22749=CARTESIAN_POINT('Ctrl Pts',(167.383432581128,-79.4297585902001,41.3983432821216));
#22750=CARTESIAN_POINT('Ctrl Pts',(168.316607594627,-79.4297719859887,41.3983383325715));
#22751=CARTESIAN_POINT('Ctrl Pts',(168.789318171633,-79.4725073961984,41.3576005032552));
#22752=CARTESIAN_POINT('Ctrl Pts',(169.704749159241,-79.6127601152316,41.1880395507574));
#22753=CARTESIAN_POINT('Ctrl Pts',(170.148057043937,-79.7078125846233,41.0590527875963));
#22754=CARTESIAN_POINT('Ctrl Pts',(170.877230469463,-79.8584385725448,40.7532327062643));
#22755=CARTESIAN_POINT('Ctrl Pts',(171.174525863015,-79.9177118275984,40.5973733005739));
#22756=CARTESIAN_POINT('Ctrl Pts',(171.45595733732,-79.9563089001744,40.4157589290663));
#22757=CARTESIAN_POINT('Ctrl Pts',(164.335473025189,-79.8042059334496,40.2771726193775));
#22758=CARTESIAN_POINT('Ctrl Pts',(164.963791192797,-79.7444108109014,40.6856055602962));
#22759=CARTESIAN_POINT('Ctrl Pts',(165.692867363639,-79.5716062994587,40.9777503392776));
#22760=CARTESIAN_POINT('Ctrl Pts',(166.924310432838,-79.4023046236385,41.221432574236));
#22761=CARTESIAN_POINT('Ctrl Pts',(167.390074212417,-79.3638725077551,41.2656132269326));
#22762=CARTESIAN_POINT('Ctrl Pts',(168.309961128106,-79.3638053779168,41.2655672039703));
#22763=CARTESIAN_POINT('Ctrl Pts',(168.775837059739,-79.4023115203605,41.2215445949071));
#22764=CARTESIAN_POINT('Ctrl Pts',(169.673734069797,-79.5257582939345,41.0435505178947));
#22765=CARTESIAN_POINT('Ctrl Pts',(170.106291243202,-79.608279307568,40.9099902338759));
#22766=CARTESIAN_POINT('Ctrl Pts',(170.811431283447,-79.7321249167481,40.6042203974311));
#22767=CARTESIAN_POINT('Ctrl Pts',(171.096853767376,-79.7785267521022,40.4510918365167));
#22768=CARTESIAN_POINT('Ctrl Pts',(171.364526974811,-79.8042059334496,40.2771726193775));
#22769=CARTESIAN_POINT('Ctrl Pts',(164.426903387699,-79.6521029667248,40.1385863096888));
#22770=CARTESIAN_POINT('Ctrl Pts',(165.023200759689,-79.6212831507678,40.5285536883552));
#22771=CARTESIAN_POINT('Ctrl Pts',(165.730469399245,-79.4781267398763,40.8301615232528));
#22772=CARTESIAN_POINT('Ctrl Pts',(166.937783093536,-79.331961481472,41.0852871258424));
#22773=CARTESIAN_POINT('Ctrl Pts',(167.396796517454,-79.2976945980757,41.1327758447739));
#22774=CARTESIAN_POINT('Ctrl Pts',(168.30327953742,-79.2977749929233,41.1328046840522));
#22775=CARTESIAN_POINT('Ctrl Pts',(168.762383358537,-79.3319478756572,41.0853222698221));
#22776=CARTESIAN_POINT('Ctrl Pts',(169.642709147199,-79.4386930097327,40.8991599406581));
#22777=CARTESIAN_POINT('Ctrl Pts',(170.064506615137,-79.5085963881185,40.7608067238982));
#22778=CARTESIAN_POINT('Ctrl Pts',(170.745644981025,-79.6058293970024,40.4552714635503));
#22779=CARTESIAN_POINT('Ctrl Pts',(171.019149702356,-79.6391850754963,40.3047425325162));
#22780=CARTESIAN_POINT('Ctrl Pts',(171.273096612301,-79.6521029667248,40.1385863096887));
#22781=CARTESIAN_POINT('Ctrl Pts',(164.518333750208,-79.5,40.));
#22782=CARTESIAN_POINT('Ctrl Pts',(165.082228306696,-79.5,40.372021477681));
#22783=CARTESIAN_POINT('Ctrl Pts',(165.767925719736,-79.3851707574638,40.6826804900184));
#22784=CARTESIAN_POINT('Ctrl Pts',(166.951286896027,-79.2616483632863,40.9491722315706));
#22785=CARTESIAN_POINT('Ctrl Pts',(167.403438148744,-79.2318085156308,41.000045789585));
#22786=CARTESIAN_POINT('Ctrl Pts',(168.296633070899,-79.2318083848514,41.000033555451));
#22787=CARTESIAN_POINT('Ctrl Pts',(168.748902246643,-79.2617519998194,40.9492663614741));
#22788=CARTESIAN_POINT('Ctrl Pts',(169.611694057755,-79.3516911884357,40.7546709077954));
#22789=CARTESIAN_POINT('Ctrl Pts',(170.022740814401,-79.4090631110633,40.6117441701778));
#22790=CARTESIAN_POINT('Ctrl Pts',(170.679845795009,-79.4795157412057,40.3062591547171));
#22791=CARTESIAN_POINT('Ctrl Pts',(170.941477606716,-79.5,40.1584610684589));
#22792=CARTESIAN_POINT('Ctrl Pts',(171.181666249792,-79.5,40.));
#22793=CARTESIAN_POINT('',(171.181666249792,-79.5,40.));
#22794=CARTESIAN_POINT('',(171.45595733732,-79.9563089001744,40.4157589290663));
#22795=CARTESIAN_POINT('',(171.181666249792,-79.5,40.));
#22796=CARTESIAN_POINT('',(164.24404266268,-79.9563089001744,40.4157589290663));
#22797=CARTESIAN_POINT('Ctrl Pts',(171.45595733732,-79.9563089001744,40.4157589290663));
#22798=CARTESIAN_POINT('Ctrl Pts',(171.174525863015,-79.9177118275984,40.5973733005739));
#22799=CARTESIAN_POINT('Ctrl Pts',(170.877230469463,-79.8584385725448,40.7532327062643));
#22800=CARTESIAN_POINT('Ctrl Pts',(170.148057043937,-79.7078125846233,41.0590527875963));
#22801=CARTESIAN_POINT('Ctrl Pts',(169.704749159241,-79.6127601152316,41.1880395507574));
#22802=CARTESIAN_POINT('Ctrl Pts',(168.789318171633,-79.4725073961984,41.3576005032552));
#22803=CARTESIAN_POINT('Ctrl Pts',(168.316607594627,-79.4297719859887,41.3983383325715));
#22804=CARTESIAN_POINT('Ctrl Pts',(167.383432581128,-79.4297585902001,41.3983432821216));
#22805=CARTESIAN_POINT('Ctrl Pts',(166.910806630347,-79.4726177418242,41.3575474685077));
#22806=CARTESIAN_POINT('Ctrl Pts',(165.655411043149,-79.6645622818713,41.125231372512));
#22807=CARTESIAN_POINT('Ctrl Pts',(164.904763645791,-79.8656939616692,40.8421377709704));
#22808=CARTESIAN_POINT('Ctrl Pts',(164.24404266268,-79.9563089001744,40.4157589290663));
#22809=CARTESIAN_POINT('',(164.518333750208,-79.5,40.));
#22810=CARTESIAN_POINT('',(164.24404266268,-79.9563089001744,40.4157589290663));
#22811=CARTESIAN_POINT('Ctrl Pts',(164.518333750208,-79.5,40.));
#22812=CARTESIAN_POINT('Ctrl Pts',(165.082228306696,-79.5,40.372021477681));
#22813=CARTESIAN_POINT('Ctrl Pts',(165.767925719736,-79.3851707574638,40.6826804900184));
#22814=CARTESIAN_POINT('Ctrl Pts',(166.951286896027,-79.2616483632863,40.9491722315706));
#22815=CARTESIAN_POINT('Ctrl Pts',(167.403438148744,-79.2318085156308,41.000045789585));
#22816=CARTESIAN_POINT('Ctrl Pts',(168.296633070899,-79.2318083848514,41.000033555451));
#22817=CARTESIAN_POINT('Ctrl Pts',(168.748902246643,-79.2617519998194,40.9492663614741));
#22818=CARTESIAN_POINT('Ctrl Pts',(169.611694057755,-79.3516911884357,40.7546709077954));
#22819=CARTESIAN_POINT('Ctrl Pts',(170.022740814401,-79.4090631110633,40.6117441701778));
#22820=CARTESIAN_POINT('Ctrl Pts',(170.679845795009,-79.4795157412057,40.3062591547171));
#22821=CARTESIAN_POINT('Ctrl Pts',(170.941477606716,-79.5,40.1584610684589));
#22822=CARTESIAN_POINT('Ctrl Pts',(171.181666249792,-79.5,40.));
#22823=CARTESIAN_POINT('Ctrl Pts',(163.678669277077,-80.,40.));
#22824=CARTESIAN_POINT('Ctrl Pts',(163.859138387108,-80.,40.1490685828142));
#22825=CARTESIAN_POINT('Ctrl Pts',(164.047413162951,-79.9832757598348,40.2888692728855));
#22826=CARTESIAN_POINT('Ctrl Pts',(164.24404266268,-79.9563089001744,40.4157589290663));
#22827=CARTESIAN_POINT('Ctrl Pts',(163.78481000794,-79.8333333333333,39.8715012722646));
#22828=CARTESIAN_POINT('Ctrl Pts',(163.960687028658,-79.8333333333333,40.0167767613686));
#22829=CARTESIAN_POINT('Ctrl Pts',(164.144230322027,-79.8221838398898,40.152892198886));
#22830=CARTESIAN_POINT('Ctrl Pts',(164.335473025189,-79.8042059334496,40.2771726193775));
#22831=CARTESIAN_POINT('Ctrl Pts',(163.890950738804,-79.6666666666667,39.7430025445293));
#22832=CARTESIAN_POINT('Ctrl Pts',(164.062235670207,-79.6666666666667,39.8844849399229));
#22833=CARTESIAN_POINT('Ctrl Pts',(164.241047481102,-79.6610919199449,40.0169151248864));
#22834=CARTESIAN_POINT('Ctrl Pts',(164.426903387699,-79.6521029667248,40.1385863096888));
#22835=CARTESIAN_POINT('Ctrl Pts',(163.997091469667,-79.5,39.6145038167939));
#22836=CARTESIAN_POINT('Ctrl Pts',(164.163784311757,-79.5,39.7521931184773));
#22837=CARTESIAN_POINT('Ctrl Pts',(164.337864640177,-79.5,39.8809380508869));
#22838=CARTESIAN_POINT('Ctrl Pts',(164.518333750208,-79.5,40.));
#22839=CARTESIAN_POINT('Ctrl Pts',(164.24404266268,-79.9563089001744,40.4157589290663));
#22840=CARTESIAN_POINT('Ctrl Pts',(164.047413162951,-79.9832757598348,40.2888692728855));
#22841=CARTESIAN_POINT('Ctrl Pts',(163.859138387108,-80.,40.1490685828142));
#22842=CARTESIAN_POINT('Ctrl Pts',(163.678669277077,-80.,40.));
#22843=CARTESIAN_POINT('Ctrl Pts',(163.997091469667,-79.5,39.6145038167939));
#22844=CARTESIAN_POINT('Ctrl Pts',(164.163784311757,-79.5,39.7521931184773));
#22845=CARTESIAN_POINT('Ctrl Pts',(164.337864640177,-79.5,39.8809380508869));
#22846=CARTESIAN_POINT('Ctrl Pts',(164.518333750208,-79.5,40.));
#22847=CARTESIAN_POINT('Origin',(167.85,-79.75,34.95));
#22848=CARTESIAN_POINT('',(172.021330722923,-80.,40.));
#22849=CARTESIAN_POINT('',(171.702908530333,-79.5,39.6145038167939));
#22850=CARTESIAN_POINT('',(172.021330722923,-80.,40.));
#22851=CARTESIAN_POINT('',(172.606870229008,-79.5,38.6882730804986));
#22852=CARTESIAN_POINT('Origin',(167.85,-79.5,34.95));
#22853=CARTESIAN_POINT('',(173.,-80.,38.9972212689696));
#22854=CARTESIAN_POINT('',(172.606870229008,-79.5,38.6882730804986));
#22855=CARTESIAN_POINT('Origin',(167.85,-80.,34.95));
#22856=CARTESIAN_POINT('Ctrl Pts',(171.45595733732,-79.9563089001744,40.4157589290663));
#22857=CARTESIAN_POINT('Ctrl Pts',(171.652586837049,-79.9832757598348,40.2888692728855));
#22858=CARTESIAN_POINT('Ctrl Pts',(171.840861612892,-80.,40.1490685828142));
#22859=CARTESIAN_POINT('Ctrl Pts',(172.021330722923,-80.,40.));
#22860=CARTESIAN_POINT('Ctrl Pts',(171.364526974811,-79.8042059334496,40.2771726193775));
#22861=CARTESIAN_POINT('Ctrl Pts',(171.555769677973,-79.8221838398898,40.152892198886));
#22862=CARTESIAN_POINT('Ctrl Pts',(171.739312971342,-79.8333333333333,40.0167767613686));
#22863=CARTESIAN_POINT('Ctrl Pts',(171.91518999206,-79.8333333333333,39.8715012722646));
#22864=CARTESIAN_POINT('Ctrl Pts',(171.273096612301,-79.6521029667248,40.1385863096888));
#22865=CARTESIAN_POINT('Ctrl Pts',(171.458952518898,-79.6610919199449,40.0169151248864));
#22866=CARTESIAN_POINT('Ctrl Pts',(171.637764329793,-79.6666666666667,39.8844849399229));
#22867=CARTESIAN_POINT('Ctrl Pts',(171.809049261196,-79.6666666666667,39.7430025445293));
#22868=CARTESIAN_POINT('Ctrl Pts',(171.181666249792,-79.5,40.));
#22869=CARTESIAN_POINT('Ctrl Pts',(171.362135359823,-79.5,39.8809380508869));
#22870=CARTESIAN_POINT('Ctrl Pts',(171.536215688243,-79.5,39.7521931184773));
#22871=CARTESIAN_POINT('Ctrl Pts',(171.702908530333,-79.5,39.6145038167939));
#22872=CARTESIAN_POINT('Ctrl Pts',(172.021330722923,-80.,40.));
#22873=CARTESIAN_POINT('Ctrl Pts',(171.840861612892,-80.,40.1490685828142));
#22874=CARTESIAN_POINT('Ctrl Pts',(171.652586837049,-79.9832757598348,40.2888692728855));
#22875=CARTESIAN_POINT('Ctrl Pts',(171.45595733732,-79.9563089001744,40.4157589290663));
#22876=CARTESIAN_POINT('Ctrl Pts',(171.181666249792,-79.5,40.));
#22877=CARTESIAN_POINT('Ctrl Pts',(171.362135359823,-79.5,39.8809380508869));
#22878=CARTESIAN_POINT('Ctrl Pts',(171.536215688243,-79.5,39.7521931184773));
#22879=CARTESIAN_POINT('Ctrl Pts',(171.702908530333,-79.5,39.6145038167939));
#22880=CARTESIAN_POINT('Ctrl Pts',(173.423859320912,-79.9545698442563,38.3862048013962));
#22881=CARTESIAN_POINT('Ctrl Pts',(173.637590761883,-79.9082209948182,38.031453352118));
#22882=CARTESIAN_POINT('Ctrl Pts',(174.161182840155,-79.6758255748561,36.8926040756434));
#22883=CARTESIAN_POINT('Ctrl Pts',(174.450714954638,-79.3629293846521,34.7340491444972));
#22884=CARTESIAN_POINT('Ctrl Pts',(174.12628339776,-79.6894007116804,33.0353820059301));
#22885=CARTESIAN_POINT('Ctrl Pts',(173.695468913621,-79.8788938435096,32.0051494847125));
#22886=CARTESIAN_POINT('Ctrl Pts',(173.568618196577,-79.9231780784845,31.7540659828401));
#22887=CARTESIAN_POINT('Ctrl Pts',(173.423859320912,-79.9545698442563,31.5137951986038));
#22888=CARTESIAN_POINT('Ctrl Pts',(173.282572880608,-79.8030465628375,38.2991037253566));
#22889=CARTESIAN_POINT('Ctrl Pts',(173.486921961723,-79.7720130814336,37.9606510628592));
#22890=CARTESIAN_POINT('Ctrl Pts',(174.009109978221,-79.5855452720181,36.8638359099341));
#22891=CARTESIAN_POINT('Ctrl Pts',(174.323939769628,-79.3038896735438,34.736501924795));
#22892=CARTESIAN_POINT('Ctrl Pts',(173.974333222952,-79.596158192733,33.0659783751474));
#22893=CARTESIAN_POINT('Ctrl Pts',(173.545800607626,-79.7480856679502,32.071313990426));
#22894=CARTESIAN_POINT('Ctrl Pts',(173.421574808057,-79.7822166975021,31.8298143240271));
#22895=CARTESIAN_POINT('Ctrl Pts',(173.282572880608,-79.8030465628375,31.6008962746433));
#22896=CARTESIAN_POINT('Ctrl Pts',(173.141286440304,-79.6515232814188,38.2120026493171));
#22897=CARTESIAN_POINT('Ctrl Pts',(173.338735235185,-79.6362079133846,37.8906417628064));
#22898=CARTESIAN_POINT('Ctrl Pts',(173.855318098134,-79.494523230808,36.8350822467445));
#22899=CARTESIAN_POINT('Ctrl Pts',(174.198332784239,-79.2449563760689,34.739214009455));
#22900=CARTESIAN_POINT('Ctrl Pts',(173.821676532788,-79.5015464237554,33.0986369664091));
#22901=CARTESIAN_POINT('Ctrl Pts',(173.396335027929,-79.6176373358252,32.1369290213944));
#22902=CARTESIAN_POINT('Ctrl Pts',(173.27441952729,-79.6409613809824,31.9059666056146));
#22903=CARTESIAN_POINT('Ctrl Pts',(173.141286440304,-79.6515232814188,31.6879973506829));
#22904=CARTESIAN_POINT('Ctrl Pts',(173.,-79.5,38.1249015732775));
#22905=CARTESIAN_POINT('Ctrl Pts',(173.188066435025,-79.5,37.8198394735476));
#22906=CARTESIAN_POINT('Ctrl Pts',(173.703245236199,-79.4042429279699,36.8063140810353));
#22907=CARTESIAN_POINT('Ctrl Pts',(174.071557599229,-79.1859166649607,34.7416667897528));
#22908=CARTESIAN_POINT('Ctrl Pts',(173.669726357979,-79.408303904808,33.1292333356263));
#22909=CARTESIAN_POINT('Ctrl Pts',(173.246666721935,-79.4868291602657,32.2030935271079));
#22910=CARTESIAN_POINT('Ctrl Pts',(173.12737613877,-79.5,31.9817149468016));
#22911=CARTESIAN_POINT('Ctrl Pts',(173.,-79.5,31.7750984267225));
#22912=CARTESIAN_POINT('',(173.,-79.5,31.7750984267225));
#22913=CARTESIAN_POINT('',(173.423859320912,-79.9545698442563,31.5137951986038));
#22914=CARTESIAN_POINT('',(173.,-79.5,31.7750984267225));
#22915=CARTESIAN_POINT('',(173.423859320912,-79.9545698442563,38.3862048013962));
#22916=CARTESIAN_POINT('Ctrl Pts',(173.423859320912,-79.9545698442563,31.5137951986038));
#22917=CARTESIAN_POINT('Ctrl Pts',(173.568618196577,-79.9231780784845,31.7540659828401));
#22918=CARTESIAN_POINT('Ctrl Pts',(173.695468913621,-79.8788938435096,32.0051494847125));
#22919=CARTESIAN_POINT('Ctrl Pts',(174.12628339776,-79.6894007116804,33.0353820059301));
#22920=CARTESIAN_POINT('Ctrl Pts',(174.450714954638,-79.3629293846521,34.7340491444972));
#22921=CARTESIAN_POINT('Ctrl Pts',(174.161182840155,-79.6758255748561,36.8926040756434));
#22922=CARTESIAN_POINT('Ctrl Pts',(173.637590761883,-79.9082209948182,38.031453352118));
#22923=CARTESIAN_POINT('Ctrl Pts',(173.423859320912,-79.9545698442563,38.3862048013962));
#22924=CARTESIAN_POINT('',(173.,-79.5,38.1249015732775));
#22925=CARTESIAN_POINT('',(173.423859320912,-79.9545698442563,38.3862048013962));
#22926=CARTESIAN_POINT('Ctrl Pts',(173.,-79.5,38.1249015732775));
#22927=CARTESIAN_POINT('Ctrl Pts',(173.188066435025,-79.5,37.8198394735476));
#22928=CARTESIAN_POINT('Ctrl Pts',(173.703245236199,-79.4042429279699,36.8063140810353));
#22929=CARTESIAN_POINT('Ctrl Pts',(174.071557599229,-79.1859166649607,34.7416667897528));
#22930=CARTESIAN_POINT('Ctrl Pts',(173.669726357979,-79.408303904808,33.1292333356263));
#22931=CARTESIAN_POINT('Ctrl Pts',(173.246666721935,-79.4868291602657,32.2030935271079));
#22932=CARTESIAN_POINT('Ctrl Pts',(173.12737613877,-79.5,31.9817149468016));
#22933=CARTESIAN_POINT('Ctrl Pts',(173.,-79.5,31.7750984267225));
#22934=CARTESIAN_POINT('Ctrl Pts',(173.,-80.,38.9972212689696));
#22935=CARTESIAN_POINT('Ctrl Pts',(173.153269804814,-80.,38.8021888152602));
#22936=CARTESIAN_POINT('Ctrl Pts',(173.295884311895,-79.9823219353749,38.5986177234898));
#22937=CARTESIAN_POINT('Ctrl Pts',(173.423859320912,-79.9545698442563,38.3862048013962));
#22938=CARTESIAN_POINT('Ctrl Pts',(172.868956743003,-79.8333333333333,38.8942385394793));
#22939=CARTESIAN_POINT('Ctrl Pts',(173.018326552783,-79.8333333333333,38.7041687436251));
#22940=CARTESIAN_POINT('Ctrl Pts',(173.157177965592,-79.8215479569166,38.5057231579888));
#22941=CARTESIAN_POINT('Ctrl Pts',(173.282572880608,-79.8030465628376,38.2991037253566));
#22942=CARTESIAN_POINT('Ctrl Pts',(172.737913486005,-79.6666666666667,38.791255809989));
#22943=CARTESIAN_POINT('Ctrl Pts',(172.883383300752,-79.6666666666667,38.6061486719899));
#22944=CARTESIAN_POINT('Ctrl Pts',(173.018471619289,-79.6607739784583,38.4128285924879));
#22945=CARTESIAN_POINT('Ctrl Pts',(173.141286440304,-79.6515232814188,38.2120026493171));
#22946=CARTESIAN_POINT('Ctrl Pts',(172.606870229008,-79.5,38.6882730804986));
#22947=CARTESIAN_POINT('Ctrl Pts',(172.748440048721,-79.5,38.5081286003548));
#22948=CARTESIAN_POINT('Ctrl Pts',(172.879765272986,-79.5,38.3199340269869));
#22949=CARTESIAN_POINT('Ctrl Pts',(173.,-79.5,38.1249015732775));
#22950=CARTESIAN_POINT('Ctrl Pts',(173.423859320912,-79.9545698442563,38.3862048013962));
#22951=CARTESIAN_POINT('Ctrl Pts',(173.295884311895,-79.9823219353749,38.5986177234898));
#22952=CARTESIAN_POINT('Ctrl Pts',(173.153269804814,-80.,38.8021888152602));
#22953=CARTESIAN_POINT('Ctrl Pts',(173.,-80.,38.9972212689696));
#22954=CARTESIAN_POINT('Ctrl Pts',(172.606870229008,-79.5,38.6882730804986));
#22955=CARTESIAN_POINT('Ctrl Pts',(172.748440048721,-79.5,38.5081286003548));
#22956=CARTESIAN_POINT('Ctrl Pts',(172.879765272986,-79.5,38.3199340269869));
#22957=CARTESIAN_POINT('Ctrl Pts',(173.,-79.5,38.1249015732775));
#22958=CARTESIAN_POINT('Ctrl Pts',(173.423859320912,-79.9545698442563,31.5137951986038));
#22959=CARTESIAN_POINT('Ctrl Pts',(173.295884311895,-79.9823219353749,31.3013822765102));
#22960=CARTESIAN_POINT('Ctrl Pts',(173.153269804814,-80.,31.0978111847398));
#22961=CARTESIAN_POINT('Ctrl Pts',(173.,-80.,30.9027787310303));
#22962=CARTESIAN_POINT('Ctrl Pts',(173.282572880608,-79.8030465628376,31.6008962746434));
#22963=CARTESIAN_POINT('Ctrl Pts',(173.157177965592,-79.8215479569166,31.3942768420111));
#22964=CARTESIAN_POINT('Ctrl Pts',(173.018326552783,-79.8333333333333,31.1958312563749));
#22965=CARTESIAN_POINT('Ctrl Pts',(172.868956743003,-79.8333333333333,31.0057614605207));
#22966=CARTESIAN_POINT('Ctrl Pts',(173.141286440304,-79.6515232814188,31.6879973506829));
#22967=CARTESIAN_POINT('Ctrl Pts',(173.018471619289,-79.6607739784583,31.4871714075121));
#22968=CARTESIAN_POINT('Ctrl Pts',(172.883383300752,-79.6666666666667,31.29385132801));
#22969=CARTESIAN_POINT('Ctrl Pts',(172.737913486005,-79.6666666666667,31.108744190011));
#22970=CARTESIAN_POINT('Ctrl Pts',(173.,-79.5,31.7750984267225));
#22971=CARTESIAN_POINT('Ctrl Pts',(172.879765272986,-79.5,31.580065973013));
#22972=CARTESIAN_POINT('Ctrl Pts',(172.748440048721,-79.5,31.3918713996451));
#22973=CARTESIAN_POINT('Ctrl Pts',(172.606870229008,-79.5,31.2117269195013));
#22974=CARTESIAN_POINT('Ctrl Pts',(173.,-80.,30.9027787310303));
#22975=CARTESIAN_POINT('Ctrl Pts',(173.153269804814,-80.,31.0978111847398));
#22976=CARTESIAN_POINT('Ctrl Pts',(173.295884311895,-79.9823219353749,31.3013822765102));
#22977=CARTESIAN_POINT('Ctrl Pts',(173.423859320912,-79.9545698442563,31.5137951986038));
#22978=CARTESIAN_POINT('Ctrl Pts',(173.,-79.5,31.7750984267225));
#22979=CARTESIAN_POINT('Ctrl Pts',(172.879765272986,-79.5,31.580065973013));
#22980=CARTESIAN_POINT('Ctrl Pts',(172.748440048721,-79.5,31.3918713996451));
#22981=CARTESIAN_POINT('Ctrl Pts',(172.606870229008,-79.5,31.2117269195013));
#22982=CARTESIAN_POINT('Origin',(125.8,-80.,-42.));
#22983=CARTESIAN_POINT('',(173.,-80.,40.));
#22984=CARTESIAN_POINT('',(173.,-80.,-21.));
#22985=CARTESIAN_POINT('',(138.1,-80.,40.));
#22986=CARTESIAN_POINT('Origin',(173.,-78.,-21.));
#22987=CARTESIAN_POINT('',(173.423859320912,-79.9545698442563,-31.5137951986038));
#22988=CARTESIAN_POINT('Ctrl Pts',(173.423859320912,-79.9545698442563,-31.5137951986038));
#22989=CARTESIAN_POINT('Ctrl Pts',(173.295884311895,-79.9823219353749,-31.3013822765102));
#22990=CARTESIAN_POINT('Ctrl Pts',(173.153269804814,-80.,-31.0978111847398));
#22991=CARTESIAN_POINT('Ctrl Pts',(173.,-80.,-30.9027787310304));
#22992=CARTESIAN_POINT('',(173.423859320912,-79.9545698442563,-38.3862048013962));
#22993=CARTESIAN_POINT('Ctrl Pts',(173.423859320912,-79.9545698442563,-38.3862048013962));
#22994=CARTESIAN_POINT('Ctrl Pts',(173.943894783993,-79.8417972672725,-37.5230499311273));
#22995=CARTESIAN_POINT('Ctrl Pts',(174.412080939248,-79.4069780593559,-35.8280882420133));
#22996=CARTESIAN_POINT('Ctrl Pts',(174.252601993115,-79.5822812285807,-33.3779001916364));
#22997=CARTESIAN_POINT('Ctrl Pts',(173.770549629633,-79.8793881262671,-32.089231778783));
#22998=CARTESIAN_POINT('Ctrl Pts',(173.423859320912,-79.9545698442563,-31.5137951986038));
#22999=CARTESIAN_POINT('',(173.,-80.,-38.9972212689696));
#23000=CARTESIAN_POINT('Ctrl Pts',(173.,-80.,-38.9972212689696));
#23001=CARTESIAN_POINT('Ctrl Pts',(173.153269804814,-80.,-38.8021888152602));
#23002=CARTESIAN_POINT('Ctrl Pts',(173.295884311895,-79.9823219353749,-38.5986177234898));
#23003=CARTESIAN_POINT('Ctrl Pts',(173.423859320912,-79.9545698442563,-38.3862048013962));
#23004=CARTESIAN_POINT('',(173.,-80.,-40.));
#23005=CARTESIAN_POINT('',(173.,-80.,-21.));
#23006=CARTESIAN_POINT('',(175.,-78.,-40.));
#23007=CARTESIAN_POINT('Origin',(173.,-78.,-40.));
#23008=CARTESIAN_POINT('',(175.,-78.,40.));
#23009=CARTESIAN_POINT('',(175.,-78.,-21.));
#23010=CARTESIAN_POINT('Origin',(173.,-78.,40.));
#23011=CARTESIAN_POINT('Origin',(167.85,-80.,34.95));
#23012=CARTESIAN_POINT('',(161.8,-62.,34.95));
#23013=CARTESIAN_POINT('',(161.8,-80.,34.95));
#23014=CARTESIAN_POINT('Origin',(167.85,-62.,34.95));
#23015=CARTESIAN_POINT('Origin',(132.15,-79.75,34.95));
#23016=CARTESIAN_POINT('',(136.002908530333,-79.5,39.6145038167939));
#23017=CARTESIAN_POINT('',(136.321330722923,-80.,40.));
#23018=CARTESIAN_POINT('',(128.132061068702,-79.5,30.4268742285492));
#23019=CARTESIAN_POINT('Origin',(132.15,-79.5,34.95));
#23020=CARTESIAN_POINT('',(128.132061068702,-79.5,30.4268742285492));
#23021=CARTESIAN_POINT('Ctrl Pts',(127.441253216958,-79.9675621326039,30.3984720929491));
#23022=CARTESIAN_POINT('Ctrl Pts',(127.010949285711,-79.8891045588851,30.8509787580965));
#23023=CARTESIAN_POINT('Ctrl Pts',(126.359829906089,-79.505173748897,31.8485409396476));
#23024=CARTESIAN_POINT('Ctrl Pts',(125.980839327581,-78.8803260190864,33.2693000226215));
#23025=CARTESIAN_POINT('Ctrl Pts',(125.89482908045,-78.6140190998926,34.4028408191624));
#23026=CARTESIAN_POINT('Ctrl Pts',(125.888503697217,-78.5931683273057,35.1083194295444));
#23027=CARTESIAN_POINT('Ctrl Pts',(125.923956953429,-78.7098702272533,36.1351458834427));
#23028=CARTESIAN_POINT('Ctrl Pts',(126.144405087748,-79.2432835801445,37.4747106349361));
#23029=CARTESIAN_POINT('Ctrl Pts',(126.667036945875,-79.6927084333072,38.5244922950161));
#23030=CARTESIAN_POINT('Ctrl Pts',(127.151416515836,-79.8969423996626,39.177231226563));
#23031=CARTESIAN_POINT('Ctrl Pts',(127.289669164758,-79.9399237215032,39.3421224520473));
#23032=CARTESIAN_POINT('Ctrl Pts',(127.441253216958,-79.9675621326039,39.5015279070509));
#23033=CARTESIAN_POINT('Ctrl Pts',(127.560835477972,-79.8117080884026,30.5140616591908));
#23034=CARTESIAN_POINT('Ctrl Pts',(127.154974662842,-79.7602628230784,30.9380771467348));
#23035=CARTESIAN_POINT('Ctrl Pts',(126.505755059624,-79.4351002932416,31.8909513534322));
#23036=CARTESIAN_POINT('Ctrl Pts',(126.07741695658,-78.8533419955133,33.2824824759202));
#23037=CARTESIAN_POINT('Ctrl Pts',(125.965427423976,-78.5983678503514,34.4062520213906));
#23038=CARTESIAN_POINT('Ctrl Pts',(125.956887081345,-78.5784245844343,35.1073387341663));
#23039=CARTESIAN_POINT('Ctrl Pts',(126.004467234684,-78.6903079144387,36.1272907384385));
#23040=CARTESIAN_POINT('Ctrl Pts',(126.273693479842,-79.1962424615693,37.4481542849529));
#23041=CARTESIAN_POINT('Ctrl Pts',(126.813063908194,-79.5941607689053,38.4609627973759));
#23042=CARTESIAN_POINT('Ctrl Pts',(127.285673917206,-79.7601242813882,39.0809512291426));
#23043=CARTESIAN_POINT('Ctrl Pts',(127.417963408171,-79.7933724658796,39.2365237097017));
#23044=CARTESIAN_POINT('Ctrl Pts',(127.560835477972,-79.8117080884026,39.3859383408092));
#23045=CARTESIAN_POINT('Ctrl Pts',(127.680417738986,-79.6558540442013,30.6296512254325));
#23046=CARTESIAN_POINT('Ctrl Pts',(127.300909005748,-79.6288417358066,31.0254726966277));
#23047=CARTESIAN_POINT('Ctrl Pts',(126.651492608816,-79.3655282549205,31.9333992201126));
#23048=CARTESIAN_POINT('Ctrl Pts',(126.175369589829,-78.8255363022201,33.2958500568041));
#23049=CARTESIAN_POINT('Ctrl Pts',(126.037188345547,-78.5824120899783,34.4097905529733));
#23050=CARTESIAN_POINT('Ctrl Pts',(126.026621490162,-78.5632074329542,35.1065199042014));
#23051=CARTESIAN_POINT('Ctrl Pts',(126.085386653903,-78.6703247029404,36.1193807396987));
#23052=CARTESIAN_POINT('Ctrl Pts',(126.402558439516,-79.1492775981534,37.4214590655734));
#23053=CARTESIAN_POINT('Ctrl Pts',(126.96087633252,-79.4942962941443,38.3976021536797));
#23054=CARTESIAN_POINT('Ctrl Pts',(127.419433872465,-79.6236341102445,38.9846162323084));
#23055=CARTESIAN_POINT('Ctrl Pts',(127.546626060281,-79.6465512556236,39.1309577515217));
#23056=CARTESIAN_POINT('Ctrl Pts',(127.680417738986,-79.6558540442013,39.2703487745675));
#23057=CARTESIAN_POINT('Ctrl Pts',(127.8,-79.5,30.7452407916743));
#23058=CARTESIAN_POINT('Ctrl Pts',(127.444934382879,-79.5,31.1125710852661));
#23059=CARTESIAN_POINT('Ctrl Pts',(126.79741776235,-79.2954547992651,31.9758096338973));
#23060=CARTESIAN_POINT('Ctrl Pts',(126.271947218828,-78.798552278647,33.3090325101028));
#23061=CARTESIAN_POINT('Ctrl Pts',(126.107786689073,-78.5667608404371,34.4132017552016));
#23062=CARTESIAN_POINT('Ctrl Pts',(126.09500487429,-78.5484636900828,35.1055392088234));
#23063=CARTESIAN_POINT('Ctrl Pts',(126.165896935158,-78.6507623901258,36.1115255946945));
#23064=CARTESIAN_POINT('Ctrl Pts',(126.53184683161,-79.1022364795782,37.3949027155902));
#23065=CARTESIAN_POINT('Ctrl Pts',(127.106903294839,-79.3957486297424,38.3340726560396));
#23066=CARTESIAN_POINT('Ctrl Pts',(127.553691273835,-79.48681599197,38.8883362348881));
#23067=CARTESIAN_POINT('Ctrl Pts',(127.674920303693,-79.5,39.0253590091761));
#23068=CARTESIAN_POINT('Ctrl Pts',(127.8,-79.5,39.1547592083257));
#23069=CARTESIAN_POINT('',(127.8,-79.5,39.1547592083257));
#23070=CARTESIAN_POINT('',(127.441253216958,-79.9675621326039,39.5015279070509));
#23071=CARTESIAN_POINT('',(127.8,-79.5,39.1547592083257));
#23072=CARTESIAN_POINT('',(127.441253216958,-79.9675621326039,30.3984720929491));
#23073=CARTESIAN_POINT('Ctrl Pts',(127.441253216958,-79.9675621326039,39.5015279070509));
#23074=CARTESIAN_POINT('Ctrl Pts',(127.289669164758,-79.9399237215032,39.3421224520473));
#23075=CARTESIAN_POINT('Ctrl Pts',(127.151416515836,-79.8969423996626,39.177231226563));
#23076=CARTESIAN_POINT('Ctrl Pts',(126.667036945875,-79.6927084333072,38.5244922950161));
#23077=CARTESIAN_POINT('Ctrl Pts',(126.144405087748,-79.2432835801445,37.4747106349361));
#23078=CARTESIAN_POINT('Ctrl Pts',(125.923956953429,-78.7098702272533,36.1351458834427));
#23079=CARTESIAN_POINT('Ctrl Pts',(125.888503697217,-78.5931683273057,35.1083194295444));
#23080=CARTESIAN_POINT('Ctrl Pts',(125.89482908045,-78.6140190998926,34.4028408191624));
#23081=CARTESIAN_POINT('Ctrl Pts',(125.980839327581,-78.8803260190864,33.2693000226215));
#23082=CARTESIAN_POINT('Ctrl Pts',(126.359829906089,-79.505173748897,31.8485409396476));
#23083=CARTESIAN_POINT('Ctrl Pts',(127.010949285711,-79.8891045588851,30.8509787580965));
#23084=CARTESIAN_POINT('Ctrl Pts',(127.441253216958,-79.9675621326039,30.3984720929491));
#23085=CARTESIAN_POINT('',(127.8,-79.5,30.7452407916743));
#23086=CARTESIAN_POINT('',(127.441253216958,-79.9675621326039,30.3984720929491));
#23087=CARTESIAN_POINT('',(126.100434613226,-78.555599219619,34.950001316873));
#23088=CARTESIAN_POINT('Ctrl Pts',(127.8,-79.5,30.7452407916743));
#23089=CARTESIAN_POINT('Ctrl Pts',(127.444934382879,-79.5,31.1125710852661));
#23090=CARTESIAN_POINT('Ctrl Pts',(126.79741776235,-79.2954547992651,31.9758096338973));
#23091=CARTESIAN_POINT('Ctrl Pts',(126.271947218828,-78.798552278647,33.3090325101028));
#23092=CARTESIAN_POINT('Ctrl Pts',(126.114775132993,-78.5766283857558,34.36619639491));
#23093=CARTESIAN_POINT('Ctrl Pts',(126.100704378151,-78.5566089729325,34.829752350636));
#23094=CARTESIAN_POINT('Ctrl Pts',(126.10063677192,-78.556545254597,34.9500019294114));
#23095=CARTESIAN_POINT('Ctrl Pts',(126.10063677192,-78.556545254597,34.9500019294114));
#23096=CARTESIAN_POINT('Ctrl Pts',(126.100608073589,-78.5565182066481,35.0010469611779));
#23097=CARTESIAN_POINT('Ctrl Pts',(126.103299297984,-78.5604327138508,35.2232403619927));
#23098=CARTESIAN_POINT('Ctrl Pts',(126.165896935158,-78.6507623901258,36.1115255946945));
#23099=CARTESIAN_POINT('Ctrl Pts',(126.53184683161,-79.1022364795782,37.3949027155902));
#23100=CARTESIAN_POINT('Ctrl Pts',(127.106903294839,-79.3957486297424,38.3340726560396));
#23101=CARTESIAN_POINT('Ctrl Pts',(127.553691273835,-79.48681599197,38.8883362348881));
#23102=CARTESIAN_POINT('Ctrl Pts',(127.674920303693,-79.5,39.0253590091761));
#23103=CARTESIAN_POINT('Ctrl Pts',(127.8,-79.5,39.1547592083257));
#23104=CARTESIAN_POINT('Ctrl Pts',(127.8,-80.,30.0530621813219));
#23105=CARTESIAN_POINT('Ctrl Pts',(127.675853962606,-80.,30.1633423773672));
#23106=CARTESIAN_POINT('Ctrl Pts',(127.555667352303,-79.9884233304841,30.2781544405375));
#23107=CARTESIAN_POINT('Ctrl Pts',(127.441253216958,-79.9675621326039,30.3984720929491));
#23108=CARTESIAN_POINT('Ctrl Pts',(127.910687022901,-79.8333333333333,30.1776661970643));
#23109=CARTESIAN_POINT('Ctrl Pts',(127.789699917756,-79.8333333333333,30.285140281251));
#23110=CARTESIAN_POINT('Ctrl Pts',(127.672644263207,-79.8256155536561,30.397089825568));
#23111=CARTESIAN_POINT('Ctrl Pts',(127.560835477972,-79.8117080884026,30.5140616591908));
#23112=CARTESIAN_POINT('Ctrl Pts',(128.021374045802,-79.6666666666667,30.3022702128068));
#23113=CARTESIAN_POINT('Ctrl Pts',(127.903545872906,-79.6666666666667,30.4069381851348));
#23114=CARTESIAN_POINT('Ctrl Pts',(127.789621174111,-79.662807776828,30.5160252105985));
#23115=CARTESIAN_POINT('Ctrl Pts',(127.680417738986,-79.6558540442013,30.6296512254325));
#23116=CARTESIAN_POINT('Ctrl Pts',(128.132061068702,-79.5,30.4268742285492));
#23117=CARTESIAN_POINT('Ctrl Pts',(128.017391828056,-79.5,30.5287360890186));
#23118=CARTESIAN_POINT('Ctrl Pts',(127.906598085016,-79.5,30.634960595629));
#23119=CARTESIAN_POINT('Ctrl Pts',(127.8,-79.5,30.7452407916743));
#23120=CARTESIAN_POINT('Ctrl Pts',(127.441253216958,-79.9675621326039,30.3984720929491));
#23121=CARTESIAN_POINT('Ctrl Pts',(127.555667352303,-79.9884233304841,30.2781544405375));
#23122=CARTESIAN_POINT('Ctrl Pts',(127.675853962606,-80.,30.1633423773672));
#23123=CARTESIAN_POINT('Ctrl Pts',(127.8,-80.,30.0530621813219));
#23124=CARTESIAN_POINT('Ctrl Pts',(128.132061068702,-79.5,30.4268742285492));
#23125=CARTESIAN_POINT('Ctrl Pts',(128.017391828056,-79.5,30.5287360890186));
#23126=CARTESIAN_POINT('Ctrl Pts',(127.906598085016,-79.5,30.634960595629));
#23127=CARTESIAN_POINT('Ctrl Pts',(127.8,-79.5,30.7452407916743));
#23128=CARTESIAN_POINT('Origin',(132.15,-79.75,34.95));
#23129=CARTESIAN_POINT('',(127.8,-80.,39.8469378186781));
#23130=CARTESIAN_POINT('',(128.132061068702,-79.5,39.4731257714508));
#23131=CARTESIAN_POINT('',(127.8,-80.,39.8469378186781));
#23132=CARTESIAN_POINT('',(128.297091469667,-79.5,39.6145038167939));
#23133=CARTESIAN_POINT('Origin',(132.15,-79.5,34.95));
#23134=CARTESIAN_POINT('',(127.978669277077,-80.,40.));
#23135=CARTESIAN_POINT('',(128.297091469667,-79.5,39.6145038167939));
#23136=CARTESIAN_POINT('Origin',(132.15,-80.,34.95));
#23137=CARTESIAN_POINT('Ctrl Pts',(127.441253216958,-79.9675621326039,39.5015279070509));
#23138=CARTESIAN_POINT('Ctrl Pts',(127.555667352303,-79.9884233304841,39.6218455594625));
#23139=CARTESIAN_POINT('Ctrl Pts',(127.675853962606,-80.,39.7366576226328));
#23140=CARTESIAN_POINT('Ctrl Pts',(127.8,-80.,39.8469378186781));
#23141=CARTESIAN_POINT('Ctrl Pts',(127.560835477972,-79.8117080884026,39.3859383408092));
#23142=CARTESIAN_POINT('Ctrl Pts',(127.672644263207,-79.8256155536561,39.502910174432));
#23143=CARTESIAN_POINT('Ctrl Pts',(127.789699917756,-79.8333333333333,39.614859718749));
#23144=CARTESIAN_POINT('Ctrl Pts',(127.910687022901,-79.8333333333333,39.7223338029357));
#23145=CARTESIAN_POINT('Ctrl Pts',(127.680417738986,-79.6558540442013,39.2703487745675));
#23146=CARTESIAN_POINT('Ctrl Pts',(127.789621174111,-79.662807776828,39.3839747894015));
#23147=CARTESIAN_POINT('Ctrl Pts',(127.903545872906,-79.6666666666667,39.4930618148652));
#23148=CARTESIAN_POINT('Ctrl Pts',(128.021374045802,-79.6666666666667,39.5977297871932));
#23149=CARTESIAN_POINT('Ctrl Pts',(127.8,-79.5,39.1547592083257));
#23150=CARTESIAN_POINT('Ctrl Pts',(127.906598085016,-79.5,39.2650394043711));
#23151=CARTESIAN_POINT('Ctrl Pts',(128.017391828056,-79.5,39.3712639109814));
#23152=CARTESIAN_POINT('Ctrl Pts',(128.132061068702,-79.5,39.4731257714508));
#23153=CARTESIAN_POINT('Ctrl Pts',(127.8,-80.,39.8469378186781));
#23154=CARTESIAN_POINT('Ctrl Pts',(127.675853962606,-80.,39.7366576226328));
#23155=CARTESIAN_POINT('Ctrl Pts',(127.555667352303,-79.9884233304841,39.6218455594625));
#23156=CARTESIAN_POINT('Ctrl Pts',(127.441253216958,-79.9675621326039,39.5015279070509));
#23157=CARTESIAN_POINT('Ctrl Pts',(127.8,-79.5,39.1547592083257));
#23158=CARTESIAN_POINT('Ctrl Pts',(127.906598085016,-79.5,39.2650394043711));
#23159=CARTESIAN_POINT('Ctrl Pts',(128.017391828056,-79.5,39.3712639109814));
#23160=CARTESIAN_POINT('Ctrl Pts',(128.132061068702,-79.5,39.4731257714508));
#23161=CARTESIAN_POINT('Ctrl Pts',(128.54404266268,-79.9563089001744,40.4157589290663));
#23162=CARTESIAN_POINT('Ctrl Pts',(129.263478466491,-79.8576414856572,40.8800278303036));
#23163=CARTESIAN_POINT('Ctrl Pts',(130.510527749596,-79.5181474324866,41.3195198524985));
#23164=CARTESIAN_POINT('Ctrl Pts',(132.744228870775,-79.3603992958393,41.4617635687488));
#23165=CARTESIAN_POINT('Ctrl Pts',(134.073121497376,-79.6275582417068,41.2167183481929));
#23166=CARTESIAN_POINT('Ctrl Pts',(135.177351519555,-79.8589667197824,40.7531589114286));
#23167=CARTESIAN_POINT('Ctrl Pts',(135.474525863015,-79.9177118275984,40.597373300574));
#23168=CARTESIAN_POINT('Ctrl Pts',(135.75595733732,-79.9563089001744,40.4157589290663));
#23169=CARTESIAN_POINT('Ctrl Pts',(128.635473025189,-79.8042059334496,40.2771726193775));
#23170=CARTESIAN_POINT('Ctrl Pts',(129.319563648041,-79.7397843653748,40.7221495906837));
#23171=CARTESIAN_POINT('Ctrl Pts',(130.533213469025,-79.4441152647883,41.1796746951226));
#23172=CARTESIAN_POINT('Ctrl Pts',(132.736413250553,-79.3011545618022,41.3347921069928));
#23173=CARTESIAN_POINT('Ctrl Pts',(134.044121571737,-79.5424668480034,41.0686029938564));
#23174=CARTESIAN_POINT('Ctrl Pts',(135.111425223576,-79.732438948176,40.6038297677597));
#23175=CARTESIAN_POINT('Ctrl Pts',(135.396943415579,-79.778678001914,40.4513160090136));
#23176=CARTESIAN_POINT('Ctrl Pts',(135.664526974811,-79.8042059334496,40.2771726193775));
#23177=CARTESIAN_POINT('Ctrl Pts',(128.726903387699,-79.6521029667248,40.1385863096888));
#23178=CARTESIAN_POINT('Ctrl Pts',(129.376253487347,-79.6178571202824,40.5629593217589));
#23179=CARTESIAN_POINT('Ctrl Pts',(130.555816201489,-79.3692164847842,41.0391855198158));
#23180=CARTESIAN_POINT('Ctrl Pts',(132.728756439743,-79.2403531910525,41.2071722557424));
#23181=CARTESIAN_POINT('Ctrl Pts',(134.01444316861,-79.4556586603759,40.9185292434998));
#23182=CARTESIAN_POINT('Ctrl Pts',(135.045825549294,-79.6063925474043,40.4552855381036));
#23183=CARTESIAN_POINT('Ctrl Pts',(135.319060054152,-79.6390338256844,40.3045183600193));
#23184=CARTESIAN_POINT('Ctrl Pts',(135.573096612301,-79.6521029667248,40.1385863096888));
#23185=CARTESIAN_POINT('Ctrl Pts',(128.818333750208,-79.5,40.));
#23186=CARTESIAN_POINT('Ctrl Pts',(129.432338668897,-79.5,40.4050810821389));
#23187=CARTESIAN_POINT('Ctrl Pts',(130.578501920918,-79.2951843170859,40.8993403624398));
#23188=CARTESIAN_POINT('Ctrl Pts',(132.720940819521,-79.1811084570154,41.0802007939864));
#23189=CARTESIAN_POINT('Ctrl Pts',(133.985443242971,-79.3705672666724,40.7704138891633));
#23190=CARTESIAN_POINT('Ctrl Pts',(134.979899253315,-79.4798647757979,40.3059563944347));
#23191=CARTESIAN_POINT('Ctrl Pts',(135.241477606716,-79.5,40.1584610684589));
#23192=CARTESIAN_POINT('Ctrl Pts',(135.481666249792,-79.5,40.));
#23193=CARTESIAN_POINT('',(135.481666249792,-79.5,40.));
#23194=CARTESIAN_POINT('',(135.75595733732,-79.9563089001744,40.4157589290663));
#23195=CARTESIAN_POINT('',(135.481666249792,-79.5,40.));
#23196=CARTESIAN_POINT('',(128.54404266268,-79.9563089001744,40.4157589290663));
#23197=CARTESIAN_POINT('Ctrl Pts',(135.75595733732,-79.9563089001744,40.4157589290663));
#23198=CARTESIAN_POINT('Ctrl Pts',(135.474525863015,-79.9177118275984,40.597373300574));
#23199=CARTESIAN_POINT('Ctrl Pts',(135.177351519555,-79.8589667197824,40.7531589114286));
#23200=CARTESIAN_POINT('Ctrl Pts',(134.073121497376,-79.6275582417068,41.2167183481929));
#23201=CARTESIAN_POINT('Ctrl Pts',(132.744228870775,-79.3603992958393,41.4617635687488));
#23202=CARTESIAN_POINT('Ctrl Pts',(130.510527749596,-79.5181474324866,41.3195198524985));
#23203=CARTESIAN_POINT('Ctrl Pts',(129.263478466491,-79.8576414856572,40.8800278303036));
#23204=CARTESIAN_POINT('Ctrl Pts',(128.54404266268,-79.9563089001744,40.4157589290663));
#23205=CARTESIAN_POINT('',(128.818333750208,-79.5,40.));
#23206=CARTESIAN_POINT('',(128.54404266268,-79.9563089001744,40.4157589290663));
#23207=CARTESIAN_POINT('Ctrl Pts',(128.818333750208,-79.5,40.));
#23208=CARTESIAN_POINT('Ctrl Pts',(129.432338668897,-79.5,40.4050810821389));
#23209=CARTESIAN_POINT('Ctrl Pts',(130.578501920918,-79.2951843170859,40.8993403624398));
#23210=CARTESIAN_POINT('Ctrl Pts',(132.720940819521,-79.1811084570154,41.0802007939864));
#23211=CARTESIAN_POINT('Ctrl Pts',(133.985443242971,-79.3705672666724,40.7704138891633));
#23212=CARTESIAN_POINT('Ctrl Pts',(134.979899253315,-79.4798647757979,40.3059563944347));
#23213=CARTESIAN_POINT('Ctrl Pts',(135.241477606716,-79.5,40.1584610684589));
#23214=CARTESIAN_POINT('Ctrl Pts',(135.481666249792,-79.5,40.));
#23215=CARTESIAN_POINT('Ctrl Pts',(127.978669277077,-80.,40.));
#23216=CARTESIAN_POINT('Ctrl Pts',(128.159138387108,-80.,40.1490685828142));
#23217=CARTESIAN_POINT('Ctrl Pts',(128.347413162951,-79.9832757598348,40.2888692728855));
#23218=CARTESIAN_POINT('Ctrl Pts',(128.54404266268,-79.9563089001744,40.4157589290663));
#23219=CARTESIAN_POINT('Ctrl Pts',(128.08481000794,-79.8333333333333,39.8715012722646));
#23220=CARTESIAN_POINT('Ctrl Pts',(128.260687028658,-79.8333333333333,40.0167767613686));
#23221=CARTESIAN_POINT('Ctrl Pts',(128.444230322027,-79.8221838398899,40.152892198886));
#23222=CARTESIAN_POINT('Ctrl Pts',(128.635473025189,-79.8042059334496,40.2771726193776));
#23223=CARTESIAN_POINT('Ctrl Pts',(128.190950738804,-79.6666666666667,39.7430025445293));
#23224=CARTESIAN_POINT('Ctrl Pts',(128.362235670207,-79.6666666666667,39.8844849399229));
#23225=CARTESIAN_POINT('Ctrl Pts',(128.541047481102,-79.6610919199449,40.0169151248865));
#23226=CARTESIAN_POINT('Ctrl Pts',(128.726903387699,-79.6521029667248,40.1385863096888));
#23227=CARTESIAN_POINT('Ctrl Pts',(128.297091469667,-79.5,39.6145038167939));
#23228=CARTESIAN_POINT('Ctrl Pts',(128.463784311757,-79.5,39.7521931184773));
#23229=CARTESIAN_POINT('Ctrl Pts',(128.637864640177,-79.5,39.8809380508869));
#23230=CARTESIAN_POINT('Ctrl Pts',(128.818333750208,-79.5,40.));
#23231=CARTESIAN_POINT('Ctrl Pts',(128.54404266268,-79.9563089001744,40.4157589290663));
#23232=CARTESIAN_POINT('Ctrl Pts',(128.347413162951,-79.9832757598348,40.2888692728855));
#23233=CARTESIAN_POINT('Ctrl Pts',(128.159138387108,-80.,40.1490685828142));
#23234=CARTESIAN_POINT('Ctrl Pts',(127.978669277077,-80.,40.));
#23235=CARTESIAN_POINT('Ctrl Pts',(128.297091469667,-79.5,39.6145038167939));
#23236=CARTESIAN_POINT('Ctrl Pts',(128.463784311757,-79.5,39.7521931184773));
#23237=CARTESIAN_POINT('Ctrl Pts',(128.637864640177,-79.5,39.8809380508869));
#23238=CARTESIAN_POINT('Ctrl Pts',(128.818333750208,-79.5,40.));
#23239=CARTESIAN_POINT('Ctrl Pts',(135.75595733732,-79.9563089001744,40.4157589290663));
#23240=CARTESIAN_POINT('Ctrl Pts',(135.952586837049,-79.9832757598348,40.2888692728855));
#23241=CARTESIAN_POINT('Ctrl Pts',(136.140861612892,-80.,40.1490685828142));
#23242=CARTESIAN_POINT('Ctrl Pts',(136.321330722923,-80.,40.));
#23243=CARTESIAN_POINT('Ctrl Pts',(135.664526974811,-79.8042059334496,40.2771726193776));
#23244=CARTESIAN_POINT('Ctrl Pts',(135.855769677973,-79.8221838398899,40.152892198886));
#23245=CARTESIAN_POINT('Ctrl Pts',(136.039312971342,-79.8333333333333,40.0167767613686));
#23246=CARTESIAN_POINT('Ctrl Pts',(136.21518999206,-79.8333333333333,39.8715012722646));
#23247=CARTESIAN_POINT('Ctrl Pts',(135.573096612301,-79.6521029667248,40.1385863096888));
#23248=CARTESIAN_POINT('Ctrl Pts',(135.758952518898,-79.6610919199449,40.0169151248865));
#23249=CARTESIAN_POINT('Ctrl Pts',(135.937764329793,-79.6666666666667,39.8844849399229));
#23250=CARTESIAN_POINT('Ctrl Pts',(136.109049261197,-79.6666666666667,39.7430025445293));
#23251=CARTESIAN_POINT('Ctrl Pts',(135.481666249792,-79.5,40.));
#23252=CARTESIAN_POINT('Ctrl Pts',(135.662135359823,-79.5,39.8809380508869));
#23253=CARTESIAN_POINT('Ctrl Pts',(135.836215688243,-79.5,39.7521931184773));
#23254=CARTESIAN_POINT('Ctrl Pts',(136.002908530333,-79.5,39.6145038167939));
#23255=CARTESIAN_POINT('Ctrl Pts',(136.321330722923,-80.,40.));
#23256=CARTESIAN_POINT('Ctrl Pts',(136.140861612892,-80.,40.1490685828142));
#23257=CARTESIAN_POINT('Ctrl Pts',(135.952586837049,-79.9832757598348,40.2888692728855));
#23258=CARTESIAN_POINT('Ctrl Pts',(135.75595733732,-79.9563089001744,40.4157589290663));
#23259=CARTESIAN_POINT('Ctrl Pts',(135.481666249792,-79.5,40.));
#23260=CARTESIAN_POINT('Ctrl Pts',(135.662135359823,-79.5,39.8809380508869));
#23261=CARTESIAN_POINT('Ctrl Pts',(135.836215688243,-79.5,39.7521931184773));
#23262=CARTESIAN_POINT('Ctrl Pts',(136.002908530333,-79.5,39.6145038167939));
#23263=CARTESIAN_POINT('Origin',(125.8,-80.,-42.));
#23264=CARTESIAN_POINT('',(127.8,-80.,40.));
#23265=CARTESIAN_POINT('',(138.1,-80.,40.));
#23266=CARTESIAN_POINT('',(127.8,-80.,-21.));
#23267=CARTESIAN_POINT('Origin',(138.1,-78.,40.));
#23268=CARTESIAN_POINT('',(173.,-78.,42.));
#23269=CARTESIAN_POINT('Origin',(173.,-78.,40.));
#23270=CARTESIAN_POINT('',(127.8,-78.,42.));
#23271=CARTESIAN_POINT('',(138.1,-78.,42.));
#23272=CARTESIAN_POINT('Origin',(127.8,-78.,40.));
#23273=CARTESIAN_POINT('Origin',(132.15,-80.,34.95));
#23274=CARTESIAN_POINT('',(126.1,-62.,34.95));
#23275=CARTESIAN_POINT('',(126.1,-80.,34.95));
#23276=CARTESIAN_POINT('Origin',(132.15,-62.,34.95));
#23277=CARTESIAN_POINT('Origin',(167.85,-79.75,-34.95));
#23278=CARTESIAN_POINT('',(172.606870229008,-79.5,-38.6882730804986));
#23279=CARTESIAN_POINT('',(173.,-80.,-38.9972212689696));
#23280=CARTESIAN_POINT('',(171.702908530333,-79.5,-39.6145038167939));
#23281=CARTESIAN_POINT('Origin',(167.85,-79.5,-34.95));
#23282=CARTESIAN_POINT('',(172.021330722923,-80.,-40.));
#23283=CARTESIAN_POINT('',(171.702908530333,-79.5,-39.6145038167939));
#23284=CARTESIAN_POINT('Origin',(167.85,-80.,-34.95));
#23285=CARTESIAN_POINT('Ctrl Pts',(171.45595733732,-79.9563089001744,-40.4157589290663));
#23286=CARTESIAN_POINT('Ctrl Pts',(171.174525863015,-79.9177118275984,-40.5973733005741));
#23287=CARTESIAN_POINT('Ctrl Pts',(170.877133620805,-79.8584176853714,-40.7532400506391));
#23288=CARTESIAN_POINT('Ctrl Pts',(170.169540370025,-79.7125526259848,-41.0499532608049));
#23289=CARTESIAN_POINT('Ctrl Pts',(169.328708923034,-79.5317501944907,-41.2992260645674));
#23290=CARTESIAN_POINT('Ctrl Pts',(167.994480347266,-79.3928715097831,-41.4336284766179));
#23291=CARTESIAN_POINT('Ctrl Pts',(166.882801505965,-79.4695633321676,-41.3620613931844));
#23292=CARTESIAN_POINT('Ctrl Pts',(165.580759305438,-79.685637902348,-41.1009423825717));
#23293=CARTESIAN_POINT('Ctrl Pts',(164.783619515538,-79.8823083392865,-40.7639606049943));
#23294=CARTESIAN_POINT('Ctrl Pts',(164.24404266268,-79.9563089001744,-40.4157589290663));
#23295=CARTESIAN_POINT('Ctrl Pts',(171.364526974811,-79.8042059334496,-40.2771726193776));
#23296=CARTESIAN_POINT('Ctrl Pts',(171.096840486452,-79.7785219817075,-40.4510535247975));
#23297=CARTESIAN_POINT('Ctrl Pts',(170.811354113016,-79.7321092034511,-40.6042844297561));
#23298=CARTESIAN_POINT('Ctrl Pts',(170.127025529992,-79.6122205931232,-40.9007863045982));
#23299=CARTESIAN_POINT('Ctrl Pts',(169.306987876026,-79.4555015304909,-41.1586880147503));
#23300=CARTESIAN_POINT('Ctrl Pts',(167.992632142232,-79.3306382944245,-41.3037702678481));
#23301=CARTESIAN_POINT('Ctrl Pts',(166.896385122953,-79.3998081962153,-41.2261517187221));
#23302=CARTESIAN_POINT('Ctrl Pts',(165.620142363097,-79.5900140227366,-40.9520929972732));
#23303=CARTESIAN_POINT('Ctrl Pts',(164.848437702289,-79.7556443218945,-40.6109203734391));
#23304=CARTESIAN_POINT('Ctrl Pts',(164.335473025189,-79.8042059334496,-40.2771726193775));
#23305=CARTESIAN_POINT('Ctrl Pts',(171.273096612301,-79.6521029667248,-40.1385863096888));
#23306=CARTESIAN_POINT('Ctrl Pts',(171.019162983279,-79.6391898458909,-40.3047808442354));
#23307=CARTESIAN_POINT('Ctrl Pts',(170.745556079207,-79.6057940059781,-40.4552285335035));
#23308=CARTESIAN_POINT('Ctrl Pts',(170.084629406995,-79.5115784193021,-40.7517034972954));
#23309=CARTESIAN_POINT('Ctrl Pts',(169.28540248269,-79.3786758644581,-41.0179405613137));
#23310=CARTESIAN_POINT('Ctrl Pts',(167.990907646826,-79.2678110265308,-41.1737902675345));
#23311=CARTESIAN_POINT('Ctrl Pts',(166.910151354644,-79.3291259492015,-41.0899409156025));
#23312=CARTESIAN_POINT('Ctrl Pts',(165.659561421505,-79.4936989232242,-40.8031820113288));
#23313=CARTESIAN_POINT('Ctrl Pts',(164.914019252474,-79.626664017392,-40.4568510431595));
#23314=CARTESIAN_POINT('Ctrl Pts',(164.426903387699,-79.6521029667248,-40.1385863096888));
#23315=CARTESIAN_POINT('Ctrl Pts',(171.181666249792,-79.5,-40.));
#23316=CARTESIAN_POINT('Ctrl Pts',(170.941477606716,-79.5,-40.1584610684588));
#23317=CARTESIAN_POINT('Ctrl Pts',(170.679776571418,-79.4794855240578,-40.3062729126205));
#23318=CARTESIAN_POINT('Ctrl Pts',(170.042114566962,-79.4112463864405,-40.6025365410887));
#23319=CARTESIAN_POINT('Ctrl Pts',(169.263681435681,-79.3024272004583,-40.8774025114966));
#23320=CARTESIAN_POINT('Ctrl Pts',(167.989059441792,-79.2055778111722,-41.0439320587647));
#23321=CARTESIAN_POINT('Ctrl Pts',(166.923734971632,-79.2593708132491,-40.9540312411402));
#23322=CARTESIAN_POINT('Ctrl Pts',(165.698944479165,-79.3980750436128,-40.6543326260304));
#23323=CARTESIAN_POINT('Ctrl Pts',(164.978837439225,-79.5,-40.3038108116042));
#23324=CARTESIAN_POINT('Ctrl Pts',(164.518333750208,-79.5,-40.));
#23325=CARTESIAN_POINT('',(164.518333750209,-79.5,-40.));
#23326=CARTESIAN_POINT('',(164.24404266268,-79.9563089001744,-40.4157589290664));
#23327=CARTESIAN_POINT('',(164.518333750209,-79.5,-40.));
#23328=CARTESIAN_POINT('',(171.45595733732,-79.9563089001744,-40.4157589290663));
#23329=CARTESIAN_POINT('Ctrl Pts',(164.24404266268,-79.9563089001744,-40.4157589290663));
#23330=CARTESIAN_POINT('Ctrl Pts',(164.783619515538,-79.8823083392865,-40.7639606049943));
#23331=CARTESIAN_POINT('Ctrl Pts',(165.580759305438,-79.685637902348,-41.1009423825717));
#23332=CARTESIAN_POINT('Ctrl Pts',(166.882801505965,-79.4695633321676,-41.3620613931844));
#23333=CARTESIAN_POINT('Ctrl Pts',(167.994480347266,-79.3928715097831,-41.4336284766179));
#23334=CARTESIAN_POINT('Ctrl Pts',(169.328708923034,-79.5317501944907,-41.2992260645674));
#23335=CARTESIAN_POINT('Ctrl Pts',(170.169540370025,-79.7125526259848,-41.0499532608049));
#23336=CARTESIAN_POINT('Ctrl Pts',(170.877133620805,-79.8584176853714,-40.7532400506391));
#23337=CARTESIAN_POINT('Ctrl Pts',(171.174525863015,-79.9177118275984,-40.5973733005741));
#23338=CARTESIAN_POINT('Ctrl Pts',(171.45595733732,-79.9563089001744,-40.4157589290663));
#23339=CARTESIAN_POINT('',(171.181666249792,-79.5,-40.));
#23340=CARTESIAN_POINT('',(171.45595733732,-79.9563089001744,-40.4157589290663));
#23341=CARTESIAN_POINT('Ctrl Pts',(171.181666249792,-79.5,-40.));
#23342=CARTESIAN_POINT('Ctrl Pts',(170.941477606716,-79.5,-40.1584610684588));
#23343=CARTESIAN_POINT('Ctrl Pts',(170.679776571418,-79.4794855240578,-40.3062729126205));
#23344=CARTESIAN_POINT('Ctrl Pts',(170.042114566962,-79.4112463864405,-40.6025365410887));
#23345=CARTESIAN_POINT('Ctrl Pts',(169.263681435681,-79.3024272004583,-40.8774025114966));
#23346=CARTESIAN_POINT('Ctrl Pts',(167.989059441792,-79.2055778111722,-41.0439320587647));
#23347=CARTESIAN_POINT('Ctrl Pts',(166.923734971632,-79.2593708132491,-40.9540312411402));
#23348=CARTESIAN_POINT('Ctrl Pts',(165.698944479165,-79.3980750436128,-40.6543326260304));
#23349=CARTESIAN_POINT('Ctrl Pts',(164.978837439225,-79.5,-40.3038108116042));
#23350=CARTESIAN_POINT('Ctrl Pts',(164.518333750208,-79.5,-40.));
#23351=CARTESIAN_POINT('Ctrl Pts',(172.021330722923,-80.,-40.));
#23352=CARTESIAN_POINT('Ctrl Pts',(171.840861612892,-80.,-40.1490685828142));
#23353=CARTESIAN_POINT('Ctrl Pts',(171.652586837049,-79.9832757598348,-40.2888692728855));
#23354=CARTESIAN_POINT('Ctrl Pts',(171.45595733732,-79.9563089001744,-40.4157589290663));
#23355=CARTESIAN_POINT('Ctrl Pts',(171.91518999206,-79.8333333333333,-39.8715012722646));
#23356=CARTESIAN_POINT('Ctrl Pts',(171.739312971342,-79.8333333333333,-40.0167767613686));
#23357=CARTESIAN_POINT('Ctrl Pts',(171.555769677973,-79.8221838398899,-40.152892198886));
#23358=CARTESIAN_POINT('Ctrl Pts',(171.364526974811,-79.8042059334496,-40.2771726193776));
#23359=CARTESIAN_POINT('Ctrl Pts',(171.809049261197,-79.6666666666667,-39.7430025445293));
#23360=CARTESIAN_POINT('Ctrl Pts',(171.637764329793,-79.6666666666667,-39.8844849399229));
#23361=CARTESIAN_POINT('Ctrl Pts',(171.458952518898,-79.6610919199449,-40.0169151248865));
#23362=CARTESIAN_POINT('Ctrl Pts',(171.273096612301,-79.6521029667248,-40.1385863096888));
#23363=CARTESIAN_POINT('Ctrl Pts',(171.702908530333,-79.5,-39.6145038167939));
#23364=CARTESIAN_POINT('Ctrl Pts',(171.536215688243,-79.5,-39.7521931184773));
#23365=CARTESIAN_POINT('Ctrl Pts',(171.362135359823,-79.5,-39.8809380508869));
#23366=CARTESIAN_POINT('Ctrl Pts',(171.181666249792,-79.5,-40.));
#23367=CARTESIAN_POINT('Ctrl Pts',(171.45595733732,-79.9563089001744,-40.4157589290663));
#23368=CARTESIAN_POINT('Ctrl Pts',(171.652586837049,-79.9832757598348,-40.2888692728855));
#23369=CARTESIAN_POINT('Ctrl Pts',(171.840861612892,-80.,-40.1490685828142));
#23370=CARTESIAN_POINT('Ctrl Pts',(172.021330722923,-80.,-40.));
#23371=CARTESIAN_POINT('Ctrl Pts',(171.702908530333,-79.5,-39.6145038167939));
#23372=CARTESIAN_POINT('Ctrl Pts',(171.536215688243,-79.5,-39.7521931184773));
#23373=CARTESIAN_POINT('Ctrl Pts',(171.362135359823,-79.5,-39.8809380508869));
#23374=CARTESIAN_POINT('Ctrl Pts',(171.181666249792,-79.5,-40.));
#23375=CARTESIAN_POINT('Origin',(167.85,-79.75,-34.95));
#23376=CARTESIAN_POINT('',(163.997091469667,-79.5,-39.6145038167939));
#23377=CARTESIAN_POINT('',(163.678669277077,-80.,-40.));
#23378=CARTESIAN_POINT('',(161.8,-79.5,-34.95));
#23379=CARTESIAN_POINT('Origin',(167.85,-79.5,-34.95));
#23380=CARTESIAN_POINT('',(172.606870229008,-79.5,-31.2117269195014));
#23381=CARTESIAN_POINT('Origin',(167.85,-79.5,-34.95));
#23382=CARTESIAN_POINT('',(172.606870229008,-79.5,-31.2117269195014));
#23383=CARTESIAN_POINT('Ctrl Pts',(164.24404266268,-79.9563089001744,-40.4157589290664));
#23384=CARTESIAN_POINT('Ctrl Pts',(164.047413162951,-79.9832757598348,-40.2888692728855));
#23385=CARTESIAN_POINT('Ctrl Pts',(163.859138387108,-80.,-40.1490685828142));
#23386=CARTESIAN_POINT('Ctrl Pts',(163.678669277077,-80.,-40.));
#23387=CARTESIAN_POINT('Ctrl Pts',(164.335473025189,-79.8042059334496,-40.2771726193776));
#23388=CARTESIAN_POINT('Ctrl Pts',(164.144230322027,-79.8221838398899,-40.152892198886));
#23389=CARTESIAN_POINT('Ctrl Pts',(163.960687028658,-79.8333333333333,-40.0167767613686));
#23390=CARTESIAN_POINT('Ctrl Pts',(163.78481000794,-79.8333333333333,-39.8715012722646));
#23391=CARTESIAN_POINT('Ctrl Pts',(164.426903387699,-79.6521029667248,-40.1385863096888));
#23392=CARTESIAN_POINT('Ctrl Pts',(164.241047481102,-79.6610919199449,-40.0169151248865));
#23393=CARTESIAN_POINT('Ctrl Pts',(164.062235670207,-79.6666666666667,-39.8844849399229));
#23394=CARTESIAN_POINT('Ctrl Pts',(163.890950738804,-79.6666666666667,-39.7430025445293));
#23395=CARTESIAN_POINT('Ctrl Pts',(164.518333750209,-79.5,-40.));
#23396=CARTESIAN_POINT('Ctrl Pts',(164.337864640177,-79.5,-39.880938050887));
#23397=CARTESIAN_POINT('Ctrl Pts',(164.163784311757,-79.5,-39.7521931184773));
#23398=CARTESIAN_POINT('Ctrl Pts',(163.997091469667,-79.5,-39.6145038167939));
#23399=CARTESIAN_POINT('Ctrl Pts',(163.678669277077,-80.,-40.));
#23400=CARTESIAN_POINT('Ctrl Pts',(163.859138387108,-80.,-40.1490685828142));
#23401=CARTESIAN_POINT('Ctrl Pts',(164.047413162951,-79.9832757598348,-40.2888692728855));
#23402=CARTESIAN_POINT('Ctrl Pts',(164.24404266268,-79.9563089001744,-40.4157589290664));
#23403=CARTESIAN_POINT('Ctrl Pts',(164.518333750209,-79.5,-40.));
#23404=CARTESIAN_POINT('Ctrl Pts',(164.337864640177,-79.5,-39.880938050887));
#23405=CARTESIAN_POINT('Ctrl Pts',(164.163784311757,-79.5,-39.7521931184773));
#23406=CARTESIAN_POINT('Ctrl Pts',(163.997091469667,-79.5,-39.6145038167939));
#23407=CARTESIAN_POINT('Ctrl Pts',(173.423859320912,-79.9545698442563,-31.5137951986038));
#23408=CARTESIAN_POINT('Ctrl Pts',(173.770549629633,-79.8793881262671,-32.089231778783));
#23409=CARTESIAN_POINT('Ctrl Pts',(174.252601993115,-79.5822812285807,-33.3779001916364));
#23410=CARTESIAN_POINT('Ctrl Pts',(174.412080939248,-79.4069780593559,-35.8280882420133));
#23411=CARTESIAN_POINT('Ctrl Pts',(173.943894783993,-79.8417972672725,-37.5230499311273));
#23412=CARTESIAN_POINT('Ctrl Pts',(173.423859320912,-79.9545698442563,-38.3862048013962));
#23413=CARTESIAN_POINT('Ctrl Pts',(173.282572880608,-79.8030465628375,-31.6008962746434));
#23414=CARTESIAN_POINT('Ctrl Pts',(173.615386259174,-79.7529254175114,-32.1494660917847));
#23415=CARTESIAN_POINT('Ctrl Pts',(174.107434573101,-79.5010021055637,-33.3992547618186));
#23416=CARTESIAN_POINT('Ctrl Pts',(174.281848391946,-79.3436199687264,-35.8173556194049));
#23417=CARTESIAN_POINT('Ctrl Pts',(173.781792948457,-79.7278648448483,-37.4762489996446));
#23418=CARTESIAN_POINT('Ctrl Pts',(173.282572880608,-79.8030465628376,-38.2991037253567));
#23419=CARTESIAN_POINT('Ctrl Pts',(173.141286440304,-79.6515232814188,-31.6879973506829));
#23420=CARTESIAN_POINT('Ctrl Pts',(173.460222888715,-79.6264627087557,-32.2097004047863));
#23421=CARTESIAN_POINT('Ctrl Pts',(173.962267153088,-79.4197229825467,-33.4206093320008));
#23422=CARTESIAN_POINT('Ctrl Pts',(174.151615844645,-79.2802618780969,-35.8066229967965));
#23423=CARTESIAN_POINT('Ctrl Pts',(173.61969111292,-79.6139324224242,-37.4294480681618));
#23424=CARTESIAN_POINT('Ctrl Pts',(173.141286440304,-79.6515232814188,-38.2120026493171));
#23425=CARTESIAN_POINT('Ctrl Pts',(173.,-79.5,-31.7750984267225));
#23426=CARTESIAN_POINT('Ctrl Pts',(173.305059518256,-79.5,-32.2699347177879));
#23427=CARTESIAN_POINT('Ctrl Pts',(173.817099733074,-79.3384438595296,-33.4419639021829));
#23428=CARTESIAN_POINT('Ctrl Pts',(174.021383297343,-79.2169037874674,-35.795890374188));
#23429=CARTESIAN_POINT('Ctrl Pts',(173.457589277384,-79.5,-37.382647136679));
#23430=CARTESIAN_POINT('Ctrl Pts',(173.,-79.5,-38.1249015732775));
#23431=CARTESIAN_POINT('',(173.,-79.5,-38.1249015732775));
#23432=CARTESIAN_POINT('',(173.,-79.5,-38.1249015732775));
#23433=CARTESIAN_POINT('',(173.,-79.5,-31.7750984267225));
#23434=CARTESIAN_POINT('',(173.423859320912,-79.9545698442563,-31.5137951986038));
#23435=CARTESIAN_POINT('Ctrl Pts',(173.,-79.5,-31.7750984267225));
#23436=CARTESIAN_POINT('Ctrl Pts',(173.305059518256,-79.5,-32.2699347177879));
#23437=CARTESIAN_POINT('Ctrl Pts',(173.817099733074,-79.3384438595296,-33.4419639021829));
#23438=CARTESIAN_POINT('Ctrl Pts',(174.021383297343,-79.2169037874674,-35.795890374188));
#23439=CARTESIAN_POINT('Ctrl Pts',(173.457589277384,-79.5,-37.382647136679));
#23440=CARTESIAN_POINT('Ctrl Pts',(173.,-79.5,-38.1249015732775));
#23441=CARTESIAN_POINT('Ctrl Pts',(173.,-80.,-30.9027787310304));
#23442=CARTESIAN_POINT('Ctrl Pts',(173.153269804814,-80.,-31.0978111847398));
#23443=CARTESIAN_POINT('Ctrl Pts',(173.295884311895,-79.9823219353749,-31.3013822765102));
#23444=CARTESIAN_POINT('Ctrl Pts',(173.423859320912,-79.9545698442563,-31.5137951986038));
#23445=CARTESIAN_POINT('Ctrl Pts',(172.868956743003,-79.8333333333333,-31.0057614605207));
#23446=CARTESIAN_POINT('Ctrl Pts',(173.018326552783,-79.8333333333333,-31.1958312563749));
#23447=CARTESIAN_POINT('Ctrl Pts',(173.157177965592,-79.8215479569166,-31.3942768420112));
#23448=CARTESIAN_POINT('Ctrl Pts',(173.282572880608,-79.8030465628376,-31.6008962746434));
#23449=CARTESIAN_POINT('Ctrl Pts',(172.737913486005,-79.6666666666667,-31.108744190011));
#23450=CARTESIAN_POINT('Ctrl Pts',(172.883383300752,-79.6666666666667,-31.2938513280101));
#23451=CARTESIAN_POINT('Ctrl Pts',(173.018471619289,-79.6607739784583,-31.4871714075121));
#23452=CARTESIAN_POINT('Ctrl Pts',(173.141286440304,-79.6515232814188,-31.6879973506829));
#23453=CARTESIAN_POINT('Ctrl Pts',(172.606870229008,-79.5,-31.2117269195014));
#23454=CARTESIAN_POINT('Ctrl Pts',(172.748440048721,-79.5,-31.3918713996452));
#23455=CARTESIAN_POINT('Ctrl Pts',(172.879765272986,-79.5,-31.5800659730131));
#23456=CARTESIAN_POINT('Ctrl Pts',(173.,-79.5,-31.7750984267225));
#23457=CARTESIAN_POINT('Ctrl Pts',(172.606870229008,-79.5,-31.2117269195014));
#23458=CARTESIAN_POINT('Ctrl Pts',(172.748440048721,-79.5,-31.3918713996452));
#23459=CARTESIAN_POINT('Ctrl Pts',(172.879765272986,-79.5,-31.5800659730131));
#23460=CARTESIAN_POINT('Ctrl Pts',(173.,-79.5,-31.7750984267225));
#23461=CARTESIAN_POINT('Ctrl Pts',(173.423859320912,-79.9545698442563,-38.3862048013962));
#23462=CARTESIAN_POINT('Ctrl Pts',(173.295884311895,-79.9823219353749,-38.5986177234898));
#23463=CARTESIAN_POINT('Ctrl Pts',(173.153269804814,-80.,-38.8021888152602));
#23464=CARTESIAN_POINT('Ctrl Pts',(173.,-80.,-38.9972212689696));
#23465=CARTESIAN_POINT('Ctrl Pts',(173.282572880608,-79.8030465628376,-38.2991037253567));
#23466=CARTESIAN_POINT('Ctrl Pts',(173.157177965592,-79.8215479569166,-38.5057231579888));
#23467=CARTESIAN_POINT('Ctrl Pts',(173.018326552783,-79.8333333333333,-38.7041687436251));
#23468=CARTESIAN_POINT('Ctrl Pts',(172.868956743003,-79.8333333333333,-38.8942385394793));
#23469=CARTESIAN_POINT('Ctrl Pts',(173.141286440304,-79.6515232814188,-38.2120026493171));
#23470=CARTESIAN_POINT('Ctrl Pts',(173.018471619289,-79.6607739784583,-38.4128285924879));
#23471=CARTESIAN_POINT('Ctrl Pts',(172.883383300752,-79.6666666666667,-38.6061486719899));
#23472=CARTESIAN_POINT('Ctrl Pts',(172.737913486005,-79.6666666666667,-38.791255809989));
#23473=CARTESIAN_POINT('Ctrl Pts',(173.,-79.5,-38.1249015732775));
#23474=CARTESIAN_POINT('Ctrl Pts',(172.879765272986,-79.5,-38.3199340269869));
#23475=CARTESIAN_POINT('Ctrl Pts',(172.748440048721,-79.5,-38.5081286003548));
#23476=CARTESIAN_POINT('Ctrl Pts',(172.606870229008,-79.5,-38.6882730804986));
#23477=CARTESIAN_POINT('Ctrl Pts',(173.,-79.5,-38.1249015732775));
#23478=CARTESIAN_POINT('Ctrl Pts',(172.879765272986,-79.5,-38.3199340269869));
#23479=CARTESIAN_POINT('Ctrl Pts',(172.748440048721,-79.5,-38.5081286003548));
#23480=CARTESIAN_POINT('Ctrl Pts',(172.606870229008,-79.5,-38.6882730804986));
#23481=CARTESIAN_POINT('Origin',(167.85,-80.,-34.95));
#23482=CARTESIAN_POINT('',(161.8,-62.,-34.95));
#23483=CARTESIAN_POINT('',(161.8,-80.,-34.95));
#23484=CARTESIAN_POINT('Origin',(167.85,-62.,-34.95));
#23485=CARTESIAN_POINT('Origin',(132.15,-79.75,-34.95));
#23486=CARTESIAN_POINT('',(128.132061068702,-79.5,-30.4268742285492));
#23487=CARTESIAN_POINT('',(127.8,-80.,-30.0530621813219));
#23488=CARTESIAN_POINT('',(136.002908530333,-79.5,-39.6145038167939));
#23489=CARTESIAN_POINT('Origin',(132.15,-79.5,-34.95));
#23490=CARTESIAN_POINT('',(136.002908530333,-79.5,-39.6145038167939));
#23491=CARTESIAN_POINT('Ctrl Pts',(135.75595733732,-79.9563089001744,-40.4157589290663));
#23492=CARTESIAN_POINT('Ctrl Pts',(134.86451977282,-79.8340522106591,-40.9910246253239));
#23493=CARTESIAN_POINT('Ctrl Pts',(133.087218623523,-79.3066015901477,-41.5050220648132));
#23494=CARTESIAN_POINT('Ctrl Pts',(130.476050150785,-79.522629291586,-41.3301097614915));
#23495=CARTESIAN_POINT('Ctrl Pts',(129.138334372346,-79.8748044404976,-40.7992693932379));
#23496=CARTESIAN_POINT('Ctrl Pts',(128.54404266268,-79.9563089001744,-40.4157589290663));
#23497=CARTESIAN_POINT('Ctrl Pts',(135.664526974811,-79.8042059334496,-40.2771726193776));
#23498=CARTESIAN_POINT('Ctrl Pts',(134.816635130887,-79.7227014737727,-40.827992194093));
#23499=CARTESIAN_POINT('Ctrl Pts',(133.07704459393,-79.2522044265217,-41.3826863416403));
#23500=CARTESIAN_POINT('Ctrl Pts',(130.49676626701,-79.4479951419512,-41.1885457912196));
#23501=CARTESIAN_POINT('Ctrl Pts',(129.200734254472,-79.7498696269984,-40.6443856691878));
#23502=CARTESIAN_POINT('Ctrl Pts',(128.635473025189,-79.8042059334496,-40.2771726193776));
#23503=CARTESIAN_POINT('Ctrl Pts',(135.573096612301,-79.6521029667248,-40.1385863096888));
#23504=CARTESIAN_POINT('Ctrl Pts',(134.768750488954,-79.6113507368864,-40.6649597628621));
#23505=CARTESIAN_POINT('Ctrl Pts',(133.066870564337,-79.1978072628957,-41.2603506184674));
#23506=CARTESIAN_POINT('Ctrl Pts',(130.517482383235,-79.3733609923163,-41.0469818209476));
#23507=CARTESIAN_POINT('Ctrl Pts',(129.263134136597,-79.6249348134992,-40.4895019451377));
#23508=CARTESIAN_POINT('Ctrl Pts',(128.726903387699,-79.6521029667248,-40.1385863096888));
#23509=CARTESIAN_POINT('Ctrl Pts',(135.481666249792,-79.5,-40.));
#23510=CARTESIAN_POINT('Ctrl Pts',(134.720865847021,-79.5,-40.5019273316312));
#23511=CARTESIAN_POINT('Ctrl Pts',(133.056696534744,-79.1434100992696,-41.1380148952945));
#23512=CARTESIAN_POINT('Ctrl Pts',(130.53819849946,-79.2987268426815,-40.9054178506757));
#23513=CARTESIAN_POINT('Ctrl Pts',(129.325534018722,-79.5,-40.3346182210876));
#23514=CARTESIAN_POINT('Ctrl Pts',(128.818333750208,-79.5,-40.));
#23515=CARTESIAN_POINT('',(128.818333750208,-79.5,-40.));
#23516=CARTESIAN_POINT('',(128.54404266268,-79.9563089001744,-40.4157589290663));
#23517=CARTESIAN_POINT('',(128.818333750208,-79.5,-40.));
#23518=CARTESIAN_POINT('',(135.75595733732,-79.9563089001744,-40.4157589290663));
#23519=CARTESIAN_POINT('Ctrl Pts',(128.54404266268,-79.9563089001744,-40.4157589290663));
#23520=CARTESIAN_POINT('Ctrl Pts',(129.138334372346,-79.8748044404976,-40.7992693932379));
#23521=CARTESIAN_POINT('Ctrl Pts',(130.476050150785,-79.522629291586,-41.3301097614915));
#23522=CARTESIAN_POINT('Ctrl Pts',(133.087218623523,-79.3066015901477,-41.5050220648132));
#23523=CARTESIAN_POINT('Ctrl Pts',(134.86451977282,-79.8340522106591,-40.9910246253239));
#23524=CARTESIAN_POINT('Ctrl Pts',(135.75595733732,-79.9563089001744,-40.4157589290663));
#23525=CARTESIAN_POINT('',(135.481666249792,-79.5,-40.));
#23526=CARTESIAN_POINT('',(135.75595733732,-79.9563089001744,-40.4157589290663));
#23527=CARTESIAN_POINT('Ctrl Pts',(135.481666249792,-79.5,-40.));
#23528=CARTESIAN_POINT('Ctrl Pts',(134.720865847021,-79.5,-40.5019273316312));
#23529=CARTESIAN_POINT('Ctrl Pts',(133.056696534744,-79.1434100992696,-41.1380148952945));
#23530=CARTESIAN_POINT('Ctrl Pts',(130.53819849946,-79.2987268426815,-40.9054178506757));
#23531=CARTESIAN_POINT('Ctrl Pts',(129.325534018722,-79.5,-40.3346182210876));
#23532=CARTESIAN_POINT('Ctrl Pts',(128.818333750208,-79.5,-40.));
#23533=CARTESIAN_POINT('Ctrl Pts',(136.321330722923,-80.,-40.));
#23534=CARTESIAN_POINT('Ctrl Pts',(136.140861612892,-80.,-40.1490685828142));
#23535=CARTESIAN_POINT('Ctrl Pts',(135.952586837049,-79.9832757598348,-40.2888692728855));
#23536=CARTESIAN_POINT('Ctrl Pts',(135.75595733732,-79.9563089001744,-40.4157589290663));
#23537=CARTESIAN_POINT('Ctrl Pts',(136.21518999206,-79.8333333333333,-39.8715012722646));
#23538=CARTESIAN_POINT('Ctrl Pts',(136.039312971342,-79.8333333333333,-40.0167767613686));
#23539=CARTESIAN_POINT('Ctrl Pts',(135.855769677973,-79.8221838398898,-40.152892198886));
#23540=CARTESIAN_POINT('Ctrl Pts',(135.664526974811,-79.8042059334496,-40.2771726193775));
#23541=CARTESIAN_POINT('Ctrl Pts',(136.109049261196,-79.6666666666667,-39.7430025445293));
#23542=CARTESIAN_POINT('Ctrl Pts',(135.937764329793,-79.6666666666667,-39.8844849399229));
#23543=CARTESIAN_POINT('Ctrl Pts',(135.758952518898,-79.6610919199449,-40.0169151248865));
#23544=CARTESIAN_POINT('Ctrl Pts',(135.573096612301,-79.6521029667248,-40.1385863096888));
#23545=CARTESIAN_POINT('Ctrl Pts',(136.002908530333,-79.5,-39.6145038167939));
#23546=CARTESIAN_POINT('Ctrl Pts',(135.836215688243,-79.5,-39.7521931184773));
#23547=CARTESIAN_POINT('Ctrl Pts',(135.662135359823,-79.5,-39.8809380508869));
#23548=CARTESIAN_POINT('Ctrl Pts',(135.481666249792,-79.5,-40.));
#23549=CARTESIAN_POINT('Ctrl Pts',(135.75595733732,-79.9563089001744,-40.4157589290663));
#23550=CARTESIAN_POINT('Ctrl Pts',(135.952586837049,-79.9832757598348,-40.2888692728855));
#23551=CARTESIAN_POINT('Ctrl Pts',(136.140861612892,-80.,-40.1490685828142));
#23552=CARTESIAN_POINT('Ctrl Pts',(136.321330722923,-80.,-40.));
#23553=CARTESIAN_POINT('Ctrl Pts',(136.002908530333,-79.5,-39.6145038167939));
#23554=CARTESIAN_POINT('Ctrl Pts',(135.836215688243,-79.5,-39.7521931184773));
#23555=CARTESIAN_POINT('Ctrl Pts',(135.662135359823,-79.5,-39.8809380508869));
#23556=CARTESIAN_POINT('Ctrl Pts',(135.481666249792,-79.5,-40.));
#23557=CARTESIAN_POINT('Origin',(132.15,-79.75,-34.95));
#23558=CARTESIAN_POINT('',(127.978669277077,-80.,-40.));
#23559=CARTESIAN_POINT('',(128.297091469667,-79.5,-39.6145038167939));
#23560=CARTESIAN_POINT('',(127.978669277077,-80.,-40.));
#23561=CARTESIAN_POINT('',(128.132061068702,-79.5,-39.4731257714508));
#23562=CARTESIAN_POINT('Origin',(132.15,-79.5,-34.95));
#23563=CARTESIAN_POINT('',(127.8,-80.,-39.8469378186781));
#23564=CARTESIAN_POINT('',(128.132061068702,-79.5,-39.4731257714508));
#23565=CARTESIAN_POINT('Origin',(132.15,-80.,-34.95));
#23566=CARTESIAN_POINT('Ctrl Pts',(128.54404266268,-79.9563089001744,-40.4157589290663));
#23567=CARTESIAN_POINT('Ctrl Pts',(128.347413162951,-79.9832757598348,-40.2888692728855));
#23568=CARTESIAN_POINT('Ctrl Pts',(128.159138387108,-80.,-40.1490685828142));
#23569=CARTESIAN_POINT('Ctrl Pts',(127.978669277077,-80.,-40.));
#23570=CARTESIAN_POINT('Ctrl Pts',(128.635473025189,-79.8042059334496,-40.2771726193776));
#23571=CARTESIAN_POINT('Ctrl Pts',(128.444230322027,-79.8221838398899,-40.152892198886));
#23572=CARTESIAN_POINT('Ctrl Pts',(128.260687028658,-79.8333333333333,-40.0167767613686));
#23573=CARTESIAN_POINT('Ctrl Pts',(128.08481000794,-79.8333333333333,-39.8715012722646));
#23574=CARTESIAN_POINT('Ctrl Pts',(128.726903387699,-79.6521029667248,-40.1385863096888));
#23575=CARTESIAN_POINT('Ctrl Pts',(128.541047481102,-79.6610919199449,-40.0169151248865));
#23576=CARTESIAN_POINT('Ctrl Pts',(128.362235670207,-79.6666666666667,-39.8844849399229));
#23577=CARTESIAN_POINT('Ctrl Pts',(128.190950738804,-79.6666666666667,-39.7430025445293));
#23578=CARTESIAN_POINT('Ctrl Pts',(128.818333750208,-79.5,-40.));
#23579=CARTESIAN_POINT('Ctrl Pts',(128.637864640177,-79.5,-39.8809380508869));
#23580=CARTESIAN_POINT('Ctrl Pts',(128.463784311757,-79.5,-39.7521931184773));
#23581=CARTESIAN_POINT('Ctrl Pts',(128.297091469667,-79.5,-39.6145038167939));
#23582=CARTESIAN_POINT('Ctrl Pts',(127.978669277077,-80.,-40.));
#23583=CARTESIAN_POINT('Ctrl Pts',(128.159138387108,-80.,-40.1490685828142));
#23584=CARTESIAN_POINT('Ctrl Pts',(128.347413162951,-79.9832757598348,-40.2888692728855));
#23585=CARTESIAN_POINT('Ctrl Pts',(128.54404266268,-79.9563089001744,-40.4157589290663));
#23586=CARTESIAN_POINT('Ctrl Pts',(128.818333750208,-79.5,-40.));
#23587=CARTESIAN_POINT('Ctrl Pts',(128.637864640177,-79.5,-39.8809380508869));
#23588=CARTESIAN_POINT('Ctrl Pts',(128.463784311757,-79.5,-39.7521931184773));
#23589=CARTESIAN_POINT('Ctrl Pts',(128.297091469667,-79.5,-39.6145038167939));
#23590=CARTESIAN_POINT('Ctrl Pts',(127.441253216958,-79.9675621326039,-39.5015279070509));
#23591=CARTESIAN_POINT('Ctrl Pts',(127.289669164758,-79.9399237215032,-39.3421224520473));
#23592=CARTESIAN_POINT('Ctrl Pts',(127.151415155152,-79.8968591135527,-39.177273607699));
#23593=CARTESIAN_POINT('Ctrl Pts',(126.747822450792,-79.7272180669214,-38.6329022417233));
#23594=CARTESIAN_POINT('Ctrl Pts',(126.309241566678,-79.4002098919181,-37.8369213100636));
#23595=CARTESIAN_POINT('Ctrl Pts',(126.016731927051,-78.9348910451195,-36.7243946241636));
#23596=CARTESIAN_POINT('Ctrl Pts',(125.908910631778,-78.6594899573144,-35.7606410832674));
#23597=CARTESIAN_POINT('Ctrl Pts',(125.874564564028,-78.539222263838,-34.6737546688422));
#23598=CARTESIAN_POINT('Ctrl Pts',(125.959716424683,-78.8398710347191,-33.3757926529076));
#23599=CARTESIAN_POINT('Ctrl Pts',(126.19182965441,-79.2152610702774,-32.5114778246844));
#23600=CARTESIAN_POINT('Ctrl Pts',(126.605719238663,-79.6417913070752,-31.4720528940946));
#23601=CARTESIAN_POINT('Ctrl Pts',(126.956346564086,-79.879148811921,-30.9083988597416));
#23602=CARTESIAN_POINT('Ctrl Pts',(127.441253216958,-79.9675621326039,-30.3984720929491));
#23603=CARTESIAN_POINT('Ctrl Pts',(127.560835477972,-79.8117080884026,-39.3859383408092));
#23604=CARTESIAN_POINT('Ctrl Pts',(127.418051256897,-79.793325904393,-39.2365308900623));
#23605=CARTESIAN_POINT('Ctrl Pts',(127.285541376279,-79.7601112769345,-39.0809829743555));
#23606=CARTESIAN_POINT('Ctrl Pts',(126.892285897958,-79.6220738739707,-38.5639460493882));
#23607=CARTESIAN_POINT('Ctrl Pts',(126.445927355906,-79.3364444622307,-37.7985867380201));
#23608=CARTESIAN_POINT('Ctrl Pts',(126.117811983079,-78.9038208567144,-36.7085188864408));
#23609=CARTESIAN_POINT('Ctrl Pts',(125.984367943213,-78.641976174545,-35.7554810788007));
#23610=CARTESIAN_POINT('Ctrl Pts',(125.937829906089,-78.5264059109537,-34.675311760547));
#23611=CARTESIAN_POINT('Ctrl Pts',(126.053536439328,-78.815363072233,-33.3868639282635));
#23612=CARTESIAN_POINT('Ctrl Pts',(126.314374424777,-79.1645141230009,-32.5409073868163));
#23613=CARTESIAN_POINT('Ctrl Pts',(126.750190464145,-79.5498792003576,-31.5311694756925));
#23614=CARTESIAN_POINT('Ctrl Pts',(127.10393121897,-79.7535405122166,-30.9919480485029));
#23615=CARTESIAN_POINT('Ctrl Pts',(127.560835477972,-79.8117080884026,-30.5140616591908));
#23616=CARTESIAN_POINT('Ctrl Pts',(127.680417738986,-79.6558540442013,-39.2703487745675));
#23617=CARTESIAN_POINT('Ctrl Pts',(127.546538211555,-79.6465978171103,-39.1309505711611));
#23618=CARTESIAN_POINT('Ctrl Pts',(127.419530900695,-79.6234887330038,-38.9846663648664));
#23619=CARTESIAN_POINT('Ctrl Pts',(127.0371705816,-79.5164766117353,-38.4950640805886));
#23620=CARTESIAN_POINT('Ctrl Pts',(126.582405406193,-79.2725817140427,-37.7601742584199));
#23621=CARTESIAN_POINT('Ctrl Pts',(126.219183523991,-78.8725648656119,-36.6928083383561));
#23622=CARTESIAN_POINT('Ctrl Pts',(126.060127983946,-78.624209642852,-35.7503531124082));
#23623=CARTESIAN_POINT('Ctrl Pts',(126.001233420716,-78.5134310859227,-34.6771492579932));
#23624=CARTESIAN_POINT('Ctrl Pts',(126.147547546007,-78.7904336631507,-33.3978245371211));
#23625=CARTESIAN_POINT('Ctrl Pts',(126.436984817076,-79.1133706812403,-32.5702845288468));
#23626=CARTESIAN_POINT('Ctrl Pts',(126.894910069842,-79.4576583699608,-31.5904079306342));
#23627=CARTESIAN_POINT('Ctrl Pts',(127.252294250593,-79.6256082997044,-31.0756336801975));
#23628=CARTESIAN_POINT('Ctrl Pts',(127.680417738986,-79.6558540442013,-30.6296512254325));
#23629=CARTESIAN_POINT('Ctrl Pts',(127.8,-79.5,-39.1547592083257));
#23630=CARTESIAN_POINT('Ctrl Pts',(127.674920303693,-79.5,-39.0253590091761));
#23631=CARTESIAN_POINT('Ctrl Pts',(127.553657121821,-79.4867408963856,-38.8883757315229));
#23632=CARTESIAN_POINT('Ctrl Pts',(127.181634028765,-79.4113324187846,-38.4261078882536));
#23633=CARTESIAN_POINT('Ctrl Pts',(126.719091195421,-79.2088162843553,-37.7218396863763));
#23634=CARTESIAN_POINT('Ctrl Pts',(126.320263580019,-78.8414946772068,-36.6769326006333));
#23635=CARTESIAN_POINT('Ctrl Pts',(126.13558529538,-78.6066958600826,-35.7451931079415));
#23636=CARTESIAN_POINT('Ctrl Pts',(126.064498762777,-78.5006147330384,-34.6787063496979));
#23637=CARTESIAN_POINT('Ctrl Pts',(126.241367560652,-78.7659257006646,-33.408895812477));
#23638=CARTESIAN_POINT('Ctrl Pts',(126.559529587444,-79.0626237339638,-32.5997140909787));
#23639=CARTESIAN_POINT('Ctrl Pts',(127.039381295324,-79.3657462632432,-31.6495245122321));
#23640=CARTESIAN_POINT('Ctrl Pts',(127.399878905477,-79.5,-31.1591828689588));
#23641=CARTESIAN_POINT('Ctrl Pts',(127.8,-79.5,-30.7452407916743));
#23642=CARTESIAN_POINT('',(127.8,-79.5,-30.7452407916743));
#23643=CARTESIAN_POINT('',(127.441253216958,-79.9675621326039,-30.3984720929491));
#23644=CARTESIAN_POINT('',(127.8,-79.5,-30.7452407916743));
#23645=CARTESIAN_POINT('',(127.441253216958,-79.9675621326039,-39.5015279070509));
#23646=CARTESIAN_POINT('Ctrl Pts',(127.441253216958,-79.9675621326039,-30.3984720929491));
#23647=CARTESIAN_POINT('Ctrl Pts',(126.956346564086,-79.879148811921,-30.9083988597416));
#23648=CARTESIAN_POINT('Ctrl Pts',(126.605719238663,-79.6417913070752,-31.4720528940946));
#23649=CARTESIAN_POINT('Ctrl Pts',(126.19182965441,-79.2152610702774,-32.5114778246844));
#23650=CARTESIAN_POINT('Ctrl Pts',(125.959716424683,-78.8398710347191,-33.3757926529076));
#23651=CARTESIAN_POINT('Ctrl Pts',(125.874564564028,-78.539222263838,-34.6737546688422));
#23652=CARTESIAN_POINT('Ctrl Pts',(125.908910631778,-78.6594899573144,-35.7606410832674));
#23653=CARTESIAN_POINT('Ctrl Pts',(126.016731927051,-78.9348910451195,-36.7243946241636));
#23654=CARTESIAN_POINT('Ctrl Pts',(126.309241566678,-79.4002098919181,-37.8369213100636));
#23655=CARTESIAN_POINT('Ctrl Pts',(126.747822450792,-79.7272180669214,-38.6329022417233));
#23656=CARTESIAN_POINT('Ctrl Pts',(127.151415155152,-79.8968591135527,-39.177273607699));
#23657=CARTESIAN_POINT('Ctrl Pts',(127.289669164758,-79.9399237215032,-39.3421224520473));
#23658=CARTESIAN_POINT('Ctrl Pts',(127.441253216958,-79.9675621326039,-39.5015279070509));
#23659=CARTESIAN_POINT('',(127.8,-79.5,-39.1547592083257));
#23660=CARTESIAN_POINT('',(127.441253216958,-79.9675621326039,-39.5015279070509));
#23661=CARTESIAN_POINT('',(126.099985641713,-78.5536625203857,-34.9499999997728));
#23662=CARTESIAN_POINT('Ctrl Pts',(127.8,-79.5,-39.1547592083257));
#23663=CARTESIAN_POINT('Ctrl Pts',(127.674920303693,-79.5,-39.0253590091761));
#23664=CARTESIAN_POINT('Ctrl Pts',(127.553657121821,-79.4867408963856,-38.8883757315229));
#23665=CARTESIAN_POINT('Ctrl Pts',(127.181634028765,-79.4113324187846,-38.4261078882536));
#23666=CARTESIAN_POINT('Ctrl Pts',(126.719091195421,-79.2088162843553,-37.7218396863763));
#23667=CARTESIAN_POINT('Ctrl Pts',(126.320263580019,-78.8414946772068,-36.6769326006333));
#23668=CARTESIAN_POINT('Ctrl Pts',(126.135611810772,-78.6067295715856,-35.7453268834825));
#23669=CARTESIAN_POINT('Ctrl Pts',(126.100062446419,-78.5536857633005,-35.2122559673255));
#23670=CARTESIAN_POINT('Ctrl Pts',(126.099985641713,-78.5536625203857,-34.9499999997728));
#23671=CARTESIAN_POINT('Ctrl Pts',(126.099985641713,-78.5536625203857,-34.9499999997728));
#23672=CARTESIAN_POINT('Ctrl Pts',(126.099985597579,-78.5536625070295,-34.9498492984475));
#23673=CARTESIAN_POINT('Ctrl Pts',(126.099852207044,-78.5536464527083,-34.4248900938296));
#23674=CARTESIAN_POINT('Ctrl Pts',(126.241367560652,-78.7659257006646,-33.408895812477));
#23675=CARTESIAN_POINT('Ctrl Pts',(126.559529587444,-79.0626237339638,-32.5997140909787));
#23676=CARTESIAN_POINT('Ctrl Pts',(127.039381295324,-79.3657462632432,-31.6495245122321));
#23677=CARTESIAN_POINT('Ctrl Pts',(127.399878905477,-79.5,-31.1591828689588));
#23678=CARTESIAN_POINT('Ctrl Pts',(127.8,-79.5,-30.7452407916743));
#23679=CARTESIAN_POINT('Ctrl Pts',(127.8,-80.,-39.8469378186781));
#23680=CARTESIAN_POINT('Ctrl Pts',(127.675853962606,-80.,-39.7366576226328));
#23681=CARTESIAN_POINT('Ctrl Pts',(127.555667352303,-79.9884233304841,-39.6218455594625));
#23682=CARTESIAN_POINT('Ctrl Pts',(127.441253216958,-79.9675621326039,-39.5015279070509));
#23683=CARTESIAN_POINT('Ctrl Pts',(127.910687022901,-79.8333333333333,-39.7223338029357));
#23684=CARTESIAN_POINT('Ctrl Pts',(127.789699917756,-79.8333333333333,-39.614859718749));
#23685=CARTESIAN_POINT('Ctrl Pts',(127.672644263207,-79.8256155536561,-39.502910174432));
#23686=CARTESIAN_POINT('Ctrl Pts',(127.560835477972,-79.8117080884026,-39.3859383408092));
#23687=CARTESIAN_POINT('Ctrl Pts',(128.021374045802,-79.6666666666667,-39.5977297871932));
#23688=CARTESIAN_POINT('Ctrl Pts',(127.903545872906,-79.6666666666667,-39.4930618148652));
#23689=CARTESIAN_POINT('Ctrl Pts',(127.789621174111,-79.662807776828,-39.3839747894015));
#23690=CARTESIAN_POINT('Ctrl Pts',(127.680417738986,-79.6558540442013,-39.2703487745675));
#23691=CARTESIAN_POINT('Ctrl Pts',(128.132061068702,-79.5,-39.4731257714508));
#23692=CARTESIAN_POINT('Ctrl Pts',(128.017391828056,-79.5,-39.3712639109814));
#23693=CARTESIAN_POINT('Ctrl Pts',(127.906598085016,-79.5,-39.2650394043711));
#23694=CARTESIAN_POINT('Ctrl Pts',(127.8,-79.5,-39.1547592083257));
#23695=CARTESIAN_POINT('Ctrl Pts',(127.441253216958,-79.9675621326039,-39.5015279070509));
#23696=CARTESIAN_POINT('Ctrl Pts',(127.555667352303,-79.9884233304841,-39.6218455594625));
#23697=CARTESIAN_POINT('Ctrl Pts',(127.675853962606,-80.,-39.7366576226328));
#23698=CARTESIAN_POINT('Ctrl Pts',(127.8,-80.,-39.8469378186781));
#23699=CARTESIAN_POINT('Ctrl Pts',(128.132061068702,-79.5,-39.4731257714508));
#23700=CARTESIAN_POINT('Ctrl Pts',(128.017391828056,-79.5,-39.3712639109814));
#23701=CARTESIAN_POINT('Ctrl Pts',(127.906598085016,-79.5,-39.2650394043711));
#23702=CARTESIAN_POINT('Ctrl Pts',(127.8,-79.5,-39.1547592083257));
#23703=CARTESIAN_POINT('Ctrl Pts',(127.441253216958,-79.9675621326039,-30.3984720929491));
#23704=CARTESIAN_POINT('Ctrl Pts',(127.555667352303,-79.9884233304841,-30.2781544405375));
#23705=CARTESIAN_POINT('Ctrl Pts',(127.675853962606,-80.,-30.1633423773672));
#23706=CARTESIAN_POINT('Ctrl Pts',(127.8,-80.,-30.0530621813219));
#23707=CARTESIAN_POINT('Ctrl Pts',(127.560835477972,-79.8117080884026,-30.5140616591908));
#23708=CARTESIAN_POINT('Ctrl Pts',(127.672644263207,-79.8256155536561,-30.397089825568));
#23709=CARTESIAN_POINT('Ctrl Pts',(127.789699917756,-79.8333333333333,-30.285140281251));
#23710=CARTESIAN_POINT('Ctrl Pts',(127.910687022901,-79.8333333333333,-30.1776661970643));
#23711=CARTESIAN_POINT('Ctrl Pts',(127.680417738986,-79.6558540442013,-30.6296512254325));
#23712=CARTESIAN_POINT('Ctrl Pts',(127.789621174111,-79.662807776828,-30.5160252105985));
#23713=CARTESIAN_POINT('Ctrl Pts',(127.903545872906,-79.6666666666667,-30.4069381851348));
#23714=CARTESIAN_POINT('Ctrl Pts',(128.021374045802,-79.6666666666667,-30.3022702128068));
#23715=CARTESIAN_POINT('Ctrl Pts',(127.8,-79.5,-30.7452407916743));
#23716=CARTESIAN_POINT('Ctrl Pts',(127.906598085016,-79.5,-30.634960595629));
#23717=CARTESIAN_POINT('Ctrl Pts',(128.017391828056,-79.5,-30.5287360890186));
#23718=CARTESIAN_POINT('Ctrl Pts',(128.132061068702,-79.5,-30.4268742285492));
#23719=CARTESIAN_POINT('Ctrl Pts',(127.8,-80.,-30.0530621813219));
#23720=CARTESIAN_POINT('Ctrl Pts',(127.675853962606,-80.,-30.1633423773672));
#23721=CARTESIAN_POINT('Ctrl Pts',(127.555667352303,-79.9884233304841,-30.2781544405375));
#23722=CARTESIAN_POINT('Ctrl Pts',(127.441253216958,-79.9675621326039,-30.3984720929491));
#23723=CARTESIAN_POINT('Ctrl Pts',(127.8,-79.5,-30.7452407916743));
#23724=CARTESIAN_POINT('Ctrl Pts',(127.906598085016,-79.5,-30.634960595629));
#23725=CARTESIAN_POINT('Ctrl Pts',(128.017391828056,-79.5,-30.5287360890186));
#23726=CARTESIAN_POINT('Ctrl Pts',(128.132061068702,-79.5,-30.4268742285492));
#23727=CARTESIAN_POINT('Origin',(125.8,-80.,-42.));
#23728=CARTESIAN_POINT('',(127.8,-80.,-40.));
#23729=CARTESIAN_POINT('',(127.8,-80.,-21.));
#23730=CARTESIAN_POINT('',(138.1,-80.,-40.));
#23731=CARTESIAN_POINT('Origin',(127.8,-78.,-21.));
#23732=CARTESIAN_POINT('',(125.8,-78.,40.));
#23733=CARTESIAN_POINT('Origin',(127.8,-78.,40.));
#23734=CARTESIAN_POINT('',(125.8,-78.,-40.));
#23735=CARTESIAN_POINT('',(125.8,-78.,-21.));
#23736=CARTESIAN_POINT('Origin',(127.8,-78.,-40.));
#23737=CARTESIAN_POINT('Origin',(132.15,-80.,-34.95));
#23738=CARTESIAN_POINT('',(126.1,-62.,-34.95));
#23739=CARTESIAN_POINT('',(126.1,-80.,-34.95));
#23740=CARTESIAN_POINT('Origin',(132.15,-62.,-34.95));
#23741=CARTESIAN_POINT('Ctrl Pts',(172.66998797436,-54.6177973391537,-42.11123563516));
#23742=CARTESIAN_POINT('Ctrl Pts',(172.674080622603,-54.619644562519,-42.1144831050407));
#23743=CARTESIAN_POINT('Ctrl Pts',(172.678173128461,-54.6215008410306,-42.1177253206949));
#23744=CARTESIAN_POINT('Ctrl Pts',(172.682265412335,-54.6233661469982,-42.1209622367086));
#23745=CARTESIAN_POINT('Ctrl Pts',(172.89432770979,-54.5345306308824,-41.8799969243272));
#23746=CARTESIAN_POINT('Ctrl Pts',(172.898404757568,-54.5364306414694,-41.8832527980149));
#23747=CARTESIAN_POINT('Ctrl Pts',(172.902480959001,-54.5383400353523,-41.8865042916576));
#23748=CARTESIAN_POINT('Ctrl Pts',(172.906556234951,-54.540258782111,-41.8897513603237));
#23749=CARTESIAN_POINT('Ctrl Pts',(173.11866744522,-54.4512639226111,-41.6487582134943));
#23750=CARTESIAN_POINT('Ctrl Pts',(173.122728892534,-54.4532167204199,-41.6520224909892));
#23751=CARTESIAN_POINT('Ctrl Pts',(173.126788789542,-54.455179229674,-41.6552832626203));
#23752=CARTESIAN_POINT('Ctrl Pts',(173.130847057568,-54.4571514172237,-41.6585404839387));
#23753=CARTESIAN_POINT('Ctrl Pts',(173.343007180649,-54.3679972143398,-41.4175195026615));
#23754=CARTESIAN_POINT('Ctrl Pts',(173.347053027499,-54.3700027993703,-41.4207921839634));
#23755=CARTESIAN_POINT('Ctrl Pts',(173.351096620082,-54.3720184239957,-41.424062233583));
#23756=CARTESIAN_POINT('Ctrl Pts',(173.355137880184,-54.3740440523364,-41.4273296075537));
#23757=CARTESIAN_POINT('',(173.343007180649,-54.3679972143398,-41.4175195026615));
#23758=CARTESIAN_POINT('',(172.66998797436,-54.6177973391537,-42.11123563516));
#23759=CARTESIAN_POINT('Ctrl Pts',(173.343007180649,-54.3679972143398,-41.4175195026615));
#23760=CARTESIAN_POINT('Ctrl Pts',(173.11866744522,-54.4512639226111,-41.6487582134943));
#23761=CARTESIAN_POINT('Ctrl Pts',(172.89432770979,-54.5345306308824,-41.8799969243272));
#23762=CARTESIAN_POINT('Ctrl Pts',(172.66998797436,-54.6177973391537,-42.11123563516));
#23763=CARTESIAN_POINT('',(173.355137880184,-54.3740440523365,-41.4273296075537));
#23764=CARTESIAN_POINT('Ctrl Pts',(173.343007180649,-54.3679972143398,-41.4175195026615));
#23765=CARTESIAN_POINT('Ctrl Pts',(173.347053027499,-54.3700027993703,-41.4207921839634));
#23766=CARTESIAN_POINT('Ctrl Pts',(173.351096620082,-54.3720184239957,-41.424062233583));
#23767=CARTESIAN_POINT('Ctrl Pts',(173.355137880184,-54.3740440523364,-41.4273296075537));
#23768=CARTESIAN_POINT('',(172.682265412335,-54.6233661469982,-42.1209622367086));
#23769=CARTESIAN_POINT('Ctrl Pts',(173.355137880184,-54.3740440523364,-41.4273296075537));
#23770=CARTESIAN_POINT('Ctrl Pts',(173.130847057568,-54.4571514172237,-41.6585404839387));
#23771=CARTESIAN_POINT('Ctrl Pts',(172.906556234951,-54.540258782111,-41.8897513603237));
#23772=CARTESIAN_POINT('Ctrl Pts',(172.682265412335,-54.6233661469982,-42.1209622367086));
#23773=CARTESIAN_POINT('Ctrl Pts',(172.682265412346,-54.6233661470033,-42.1209622367175));
#23774=CARTESIAN_POINT('Ctrl Pts',(172.678173128469,-54.6215008410342,-42.1177253207011));
#23775=CARTESIAN_POINT('Ctrl Pts',(172.674080622608,-54.619644562521,-42.1144831050443));
#23776=CARTESIAN_POINT('Ctrl Pts',(172.669987974361,-54.6177973391542,-42.1112356351609));
#23777=CARTESIAN_POINT('Ctrl Pts',(172.682265412335,-54.6233661469982,-42.1209622367086));
#23778=CARTESIAN_POINT('Ctrl Pts',(173.215637563912,-54.8664827752239,-42.5428491125249));
#23779=CARTESIAN_POINT('Ctrl Pts',(173.745325571242,-55.2614905271195,-42.8738456760892));
#23780=CARTESIAN_POINT('Ctrl Pts',(174.217811580545,-55.9131609972939,-43.079781844656));
#23781=CARTESIAN_POINT('Ctrl Pts',(174.312192137058,-56.0793965789834,-43.1103778842156));
#23782=CARTESIAN_POINT('Ctrl Pts',(174.435796016049,-56.3890168894375,-43.1269819071719));
#23783=CARTESIAN_POINT('Ctrl Pts',(174.47235407616,-56.5277138229442,-43.1199886669764));
#23784=CARTESIAN_POINT('Ctrl Pts',(174.496492816042,-56.7264202902178,-43.0887325863734));
#23785=CARTESIAN_POINT('Ctrl Pts',(174.5,-56.7847063150805,-43.076852451079));
#23786=CARTESIAN_POINT('Ctrl Pts',(174.5,-56.8425310374202,-43.0623574561495));
#23787=CARTESIAN_POINT('Ctrl Pts',(172.906556234951,-54.540258782111,-41.8897513603237));
#23788=CARTESIAN_POINT('Ctrl Pts',(173.438158459423,-54.7903069194011,-42.3123493732582));
#23789=CARTESIAN_POINT('Ctrl Pts',(173.951777237242,-55.1979783837946,-42.6621969802207));
#23790=CARTESIAN_POINT('Ctrl Pts',(174.400091244966,-55.8634829413806,-42.897229613997));
#23791=CARTESIAN_POINT('Ctrl Pts',(174.489150256805,-56.032697189635,-42.9342422759036));
#23792=CARTESIAN_POINT('Ctrl Pts',(174.605182937368,-56.3464560071092,-42.9602413169397));
#23793=CARTESIAN_POINT('Ctrl Pts',(174.639555462911,-56.4864133676013,-42.9560967838325));
#23794=CARTESIAN_POINT('Ctrl Pts',(174.662739203426,-56.6858634968676,-42.9267868754762));
#23795=CARTESIAN_POINT('Ctrl Pts',(174.666281991153,-56.7442283004779,-42.9151689331802));
#23796=CARTESIAN_POINT('Ctrl Pts',(174.666585068858,-56.8020063133375,-42.9006926242979));
#23797=CARTESIAN_POINT('Ctrl Pts',(173.130847057568,-54.4571514172237,-41.6585404839387));
#23798=CARTESIAN_POINT('Ctrl Pts',(173.659338898785,-54.7142323226278,-42.0836859927104));
#23799=CARTESIAN_POINT('Ctrl Pts',(174.157044295027,-55.1347188176983,-42.4519992190559));
#23800=CARTESIAN_POINT('Ctrl Pts',(174.582681714858,-55.8137303528632,-42.7143006025566));
#23801=CARTESIAN_POINT('Ctrl Pts',(174.665886765686,-55.9860386883128,-42.7583769624203));
#23802=CARTESIAN_POINT('Ctrl Pts',(174.77469850772,-56.3038647001878,-42.7933478117247));
#23803=CARTESIAN_POINT('Ctrl Pts',(174.806676184536,-56.4451249038791,-42.7922907429087));
#23804=CARTESIAN_POINT('Ctrl Pts',(174.829014350795,-56.6453016466416,-42.7648116347366));
#23805=CARTESIAN_POINT('Ctrl Pts',(174.83254353756,-56.7037531597607,-42.7535060960931));
#23806=CARTESIAN_POINT('Ctrl Pts',(174.833170137715,-56.7614815892548,-42.7390277924464));
#23807=CARTESIAN_POINT('Ctrl Pts',(173.355137880184,-54.3740440523364,-41.4273296075537));
#23808=CARTESIAN_POINT('Ctrl Pts',(173.881859794296,-54.6380564668049,-41.8531862534437));
#23809=CARTESIAN_POINT('Ctrl Pts',(174.363495961026,-55.0712066743734,-42.2403505231874));
#23810=CARTESIAN_POINT('Ctrl Pts',(174.76496137928,-55.7640522969499,-42.5317483718976));
#23811=CARTESIAN_POINT('Ctrl Pts',(174.842844885433,-55.9393392989643,-42.5822413541083));
#23812=CARTESIAN_POINT('Ctrl Pts',(174.944085429039,-56.2613038178594,-42.6266072214926));
#23813=CARTESIAN_POINT('Ctrl Pts',(174.973877571286,-56.4038244485362,-42.6283988597648));
#23814=CARTESIAN_POINT('Ctrl Pts',(174.995260738178,-56.6047448532914,-42.6028659238394));
#23815=CARTESIAN_POINT('Ctrl Pts',(174.998825528713,-56.663275145158,-42.5918225781943));
#23816=CARTESIAN_POINT('Ctrl Pts',(174.999755206573,-56.7209568651721,-42.5773629605948));
#23817=CARTESIAN_POINT('',(174.999755206573,-56.7209568651721,-42.5773629605948));
#23818=CARTESIAN_POINT('Ctrl Pts',(173.355137880175,-54.374044052332,-41.4273296075466));
#23819=CARTESIAN_POINT('Ctrl Pts',(173.88185979429,-54.6380564668001,-41.8531862534394));
#23820=CARTESIAN_POINT('Ctrl Pts',(174.363495961024,-55.0712066743705,-42.2403505231862));
#23821=CARTESIAN_POINT('Ctrl Pts',(174.66758815857,-55.5960064163895,-42.4610714324983));
#23822=CARTESIAN_POINT('Ctrl Pts',(174.76496137928,-55.7640522969499,-42.5317483718976));
#23823=CARTESIAN_POINT('Ctrl Pts',(174.842844885433,-55.9393392989643,-42.5822413541083));
#23824=CARTESIAN_POINT('Ctrl Pts',(174.898252534763,-56.1155463453136,-42.6065222235573));
#23825=CARTESIAN_POINT('Ctrl Pts',(174.944085429039,-56.2613038178594,-42.6266072214926));
#23826=CARTESIAN_POINT('Ctrl Pts',(174.973877571286,-56.4038244485362,-42.6283988597648));
#23827=CARTESIAN_POINT('Ctrl Pts',(174.988900500091,-56.5449828162991,-42.6104604748416));
#23828=CARTESIAN_POINT('Ctrl Pts',(174.995260738178,-56.6047448532914,-42.6028659238394));
#23829=CARTESIAN_POINT('Ctrl Pts',(174.998825528713,-56.663275145158,-42.5918225781943));
#23830=CARTESIAN_POINT('Ctrl Pts',(174.999755206573,-56.7209568651721,-42.5773629605948));
#23831=CARTESIAN_POINT('',(174.5,-56.8425310374202,-43.0623574561495));
#23832=CARTESIAN_POINT('',(174.999755206573,-56.7209568651721,-42.5773629605948));
#23833=CARTESIAN_POINT('Ctrl Pts',(174.5,-56.8425310374202,-43.0623574561495));
#23834=CARTESIAN_POINT('Ctrl Pts',(174.5,-56.7847063150805,-43.076852451079));
#23835=CARTESIAN_POINT('Ctrl Pts',(174.496492816042,-56.7264202902178,-43.0887325863734));
#23836=CARTESIAN_POINT('Ctrl Pts',(174.47235407616,-56.5277138229442,-43.1199886669764));
#23837=CARTESIAN_POINT('Ctrl Pts',(174.435796016049,-56.3890168894375,-43.1269819071719));
#23838=CARTESIAN_POINT('Ctrl Pts',(174.312192137058,-56.0793965789834,-43.1103778842156));
#23839=CARTESIAN_POINT('Ctrl Pts',(174.217811580545,-55.9131609972939,-43.079781844656));
#23840=CARTESIAN_POINT('Ctrl Pts',(173.745325571242,-55.2614905271195,-42.8738456760892));
#23841=CARTESIAN_POINT('Ctrl Pts',(173.215637563912,-54.8664827752239,-42.5428491125249));
#23842=CARTESIAN_POINT('Ctrl Pts',(172.682265412335,-54.6233661469982,-42.1209622367086));
#23843=CARTESIAN_POINT('Ctrl Pts',(172.761788838589,-54.6513921669961,-42.1680911210267));
#23844=CARTESIAN_POINT('Ctrl Pts',(172.756002505546,-54.6497207785918,-42.165366227668));
#23845=CARTESIAN_POINT('Ctrl Pts',(172.719569461485,-54.6401760230924,-42.1505779818549));
#23846=CARTESIAN_POINT('Ctrl Pts',(172.66998797436,-54.6177973391537,-42.11123563516));
#23847=CARTESIAN_POINT('Ctrl Pts',(172.922596211878,-54.5437202426897,-41.8972936159369));
#23848=CARTESIAN_POINT('Ctrl Pts',(172.921559444571,-54.5435041843234,-41.8968224784597));
#23849=CARTESIAN_POINT('Ctrl Pts',(172.910302152746,-54.5409830080962,-41.892409256866));
#23850=CARTESIAN_POINT('Ctrl Pts',(172.89432770979,-54.5345306308824,-41.8799969243272));
#23851=CARTESIAN_POINT('Ctrl Pts',(173.083403585168,-54.4360483183833,-41.6264961108471));
#23852=CARTESIAN_POINT('Ctrl Pts',(173.087116383597,-54.4372875900551,-41.6282787292514));
#23853=CARTESIAN_POINT('Ctrl Pts',(173.101034844007,-54.4417899931,-41.6342405318772));
#23854=CARTESIAN_POINT('Ctrl Pts',(173.11866744522,-54.4512639226111,-41.6487582134943));
#23855=CARTESIAN_POINT('Ctrl Pts',(173.244210958458,-54.3283763940769,-41.3556986057572));
#23856=CARTESIAN_POINT('Ctrl Pts',(173.252673322623,-54.3310709957867,-41.3597349800431));
#23857=CARTESIAN_POINT('Ctrl Pts',(173.291767535267,-54.3425969781039,-41.3760718068883));
#23858=CARTESIAN_POINT('Ctrl Pts',(173.343007180649,-54.3679972143398,-41.4175195026615));
#23859=CARTESIAN_POINT('',(172.761788838585,-54.651392166995,-42.168091121025));
#23860=CARTESIAN_POINT('Ctrl Pts',(172.669987974309,-54.6177973391308,-42.1112356351198));
#23861=CARTESIAN_POINT('Ctrl Pts',(172.719569461453,-54.6401760230827,-42.1505779818392));
#23862=CARTESIAN_POINT('Ctrl Pts',(172.756002505533,-54.6497207785884,-42.1653662276628));
#23863=CARTESIAN_POINT('Ctrl Pts',(172.761788838586,-54.6513921669954,-42.1680911210256));
#23864=CARTESIAN_POINT('',(172.95698498009,-54.520694527064,-41.8393833818205));
#23865=CARTESIAN_POINT('Ctrl Pts',(172.761788838589,-54.6513921669961,-42.1680911210267));
#23866=CARTESIAN_POINT('Ctrl Pts',(172.826854219089,-54.6078262870188,-42.0585218746247));
#23867=CARTESIAN_POINT('Ctrl Pts',(172.89191959959,-54.5642604070414,-41.9489526282227));
#23868=CARTESIAN_POINT('Ctrl Pts',(172.95698498009,-54.5206945270641,-41.8393833818207));
#23869=CARTESIAN_POINT('',(173.244210958463,-54.3283763940785,-41.3556986057596));
#23870=CARTESIAN_POINT('Ctrl Pts',(172.95698498009,-54.5206945270641,-41.8393833818207));
#23871=CARTESIAN_POINT('Ctrl Pts',(173.052726972879,-54.456588482735,-41.6781551231329));
#23872=CARTESIAN_POINT('Ctrl Pts',(173.148468965669,-54.392482438406,-41.516926864445));
#23873=CARTESIAN_POINT('Ctrl Pts',(173.244210958458,-54.3283763940769,-41.3556986057572));
#23874=CARTESIAN_POINT('Ctrl Pts',(173.244210958458,-54.3283763940769,-41.3556986057572));
#23875=CARTESIAN_POINT('Ctrl Pts',(173.252673322623,-54.3310709957867,-41.3597349800431));
#23876=CARTESIAN_POINT('Ctrl Pts',(173.291767535267,-54.3425969781039,-41.3760718068883));
#23877=CARTESIAN_POINT('Ctrl Pts',(173.343007180649,-54.3679972143398,-41.4175195026615));
#23878=CARTESIAN_POINT('Origin',(174.75,-56.3562342901464,-41.1223792414288));
#23879=CARTESIAN_POINT('',(175.,-57.351354804662,-40.));
#23880=CARTESIAN_POINT('',(174.499999999905,-58.3461592102992,-41.3228756557483));
#23881=CARTESIAN_POINT('Ctrl Pts',(174.499999999896,-58.3461592104135,-41.3228756556501));
#23882=CARTESIAN_POINT('Ctrl Pts',(174.545769052472,-58.3053873720851,-41.270978428147));
#23883=CARTESIAN_POINT('Ctrl Pts',(174.588496139891,-58.2661562974069,-41.217054380861));
#23884=CARTESIAN_POINT('Ctrl Pts',(174.701138126955,-58.1568455611625,-41.0593011894553));
#23885=CARTESIAN_POINT('Ctrl Pts',(174.776779134635,-58.0729443622281,-40.9266860356746));
#23886=CARTESIAN_POINT('Ctrl Pts',(174.86686770893,-57.9430044328017,-40.7239686970479));
#23887=CARTESIAN_POINT('Ctrl Pts',(174.904968042358,-57.8725498634399,-40.6161672831003));
#23888=CARTESIAN_POINT('Ctrl Pts',(174.957119187857,-57.7379468702121,-40.4252008690903));
#23889=CARTESIAN_POINT('Ctrl Pts',(174.978867869175,-57.6455132484847,-40.3052809972307));
#23890=CARTESIAN_POINT('Ctrl Pts',(174.996519917819,-57.4970226095956,-40.1383691282534));
#23891=CARTESIAN_POINT('Ctrl Pts',(175.,-57.4269240433684,-40.0670009716212));
#23892=CARTESIAN_POINT('Ctrl Pts',(175.,-57.351354804662,-40.));
#23893=CARTESIAN_POINT('',(174.5,-56.8829468279694,-43.0517765313875));
#23894=CARTESIAN_POINT('Origin',(174.5,-56.3562342901464,-41.1223792414288));
#23895=CARTESIAN_POINT('',(175.,-56.7512686935136,-42.5694272088978));
#23896=CARTESIAN_POINT('',(174.5,-56.8829468279694,-43.0517765313875));
#23897=CARTESIAN_POINT('Origin',(175.,-56.3562342901464,-41.1223792414288));
#23898=CARTESIAN_POINT('Ctrl Pts',(174.5,-56.8425310374202,-43.0623574561495));
#23899=CARTESIAN_POINT('Ctrl Pts',(174.5,-56.8560393157734,-43.0589713192462));
#23900=CARTESIAN_POINT('Ctrl Pts',(174.5,-56.8695122257409,-43.0554440878163));
#23901=CARTESIAN_POINT('Ctrl Pts',(174.5,-56.8829468279694,-43.0517765313875));
#23902=CARTESIAN_POINT('Ctrl Pts',(174.666585068858,-56.8020063133375,-42.9006926242979));
#23903=CARTESIAN_POINT('Ctrl Pts',(174.666639498249,-56.8143888954835,-42.8975886395879));
#23904=CARTESIAN_POINT('Ctrl Pts',(174.666666666667,-56.8267390644414,-42.8943553506173));
#23905=CARTESIAN_POINT('Ctrl Pts',(174.666666666667,-56.8390541164841,-42.890993423891));
#23906=CARTESIAN_POINT('Ctrl Pts',(174.833170137715,-56.7614815892548,-42.7390277924464));
#23907=CARTESIAN_POINT('Ctrl Pts',(174.833278996499,-56.7727384751935,-42.7362059599296));
#23908=CARTESIAN_POINT('Ctrl Pts',(174.833333333333,-56.7839659031418,-42.7332666134184));
#23909=CARTESIAN_POINT('Ctrl Pts',(174.833333333333,-56.7951614049989,-42.7302103163944));
#23910=CARTESIAN_POINT('Ctrl Pts',(174.999755206573,-56.7209568651721,-42.5773629605948));
#23911=CARTESIAN_POINT('Ctrl Pts',(174.999918494748,-56.7310880549036,-42.5748232802713));
#23912=CARTESIAN_POINT('Ctrl Pts',(175.,-56.7411927418423,-42.5721778762194));
#23913=CARTESIAN_POINT('Ctrl Pts',(175.,-56.7512686935137,-42.5694272088978));
#23914=CARTESIAN_POINT('Ctrl Pts',(174.5,-56.8829468279694,-43.0517765313875));
#23915=CARTESIAN_POINT('Ctrl Pts',(174.5,-56.8695122257409,-43.0554440878163));
#23916=CARTESIAN_POINT('Ctrl Pts',(174.5,-56.8560393157734,-43.0589713192462));
#23917=CARTESIAN_POINT('Ctrl Pts',(174.5,-56.8425310374202,-43.0623574561495));
#23918=CARTESIAN_POINT('Ctrl Pts',(174.999755206573,-56.7209568651721,-42.5773629605948));
#23919=CARTESIAN_POINT('Ctrl Pts',(174.999918494748,-56.7310880549036,-42.5748232802713));
#23920=CARTESIAN_POINT('Ctrl Pts',(175.,-56.7411927418423,-42.5721778762194));
#23921=CARTESIAN_POINT('Ctrl Pts',(175.,-56.7512686935137,-42.5694272088978));
#23922=CARTESIAN_POINT('Ctrl Pts',(172.761788838585,-54.651392166995,-42.168091121025));
#23923=CARTESIAN_POINT('Ctrl Pts',(172.841192559056,-54.574303158249,-42.0424115797416));
#23924=CARTESIAN_POINT('Ctrl Pts',(172.920596279528,-54.5111710705365,-41.908178056654));
#23925=CARTESIAN_POINT('Ctrl Pts',(173.,-54.463528575122,-41.7686493678573));
#23926=CARTESIAN_POINT('Ctrl Pts',(172.922596211877,-54.5437202426895,-41.8972936159365));
#23927=CARTESIAN_POINT('Ctrl Pts',(172.948533142216,-54.5068055874631,-41.859694919166));
#23928=CARTESIAN_POINT('Ctrl Pts',(172.97426662197,-54.4797095101407,-41.8160378311823));
#23929=CARTESIAN_POINT('Ctrl Pts',(173.,-54.463528575122,-41.7686493678573));
#23930=CARTESIAN_POINT('Ctrl Pts',(173.08340358517,-54.436048318384,-41.6264961108481));
#23931=CARTESIAN_POINT('Ctrl Pts',(173.055873725375,-54.4393080166772,-41.6769782585905));
#23932=CARTESIAN_POINT('Ctrl Pts',(173.027936964413,-54.4482479497449,-41.7238976057107));
#23933=CARTESIAN_POINT('Ctrl Pts',(173.,-54.463528575122,-41.7686493678573));
#23934=CARTESIAN_POINT('Ctrl Pts',(173.244210958463,-54.3283763940785,-41.3556986057596));
#23935=CARTESIAN_POINT('Ctrl Pts',(173.163214308534,-54.3718104458914,-41.494261598015));
#23936=CARTESIAN_POINT('Ctrl Pts',(173.081607306855,-54.4167863893491,-41.631757380239));
#23937=CARTESIAN_POINT('Ctrl Pts',(173.,-54.463528575122,-41.7686493678573));
#23938=CARTESIAN_POINT('',(173.,-54.463528575122,-41.7686493678573));
#23939=CARTESIAN_POINT('Ctrl Pts',(172.761788838585,-54.651392166995,-42.168091121025));
#23940=CARTESIAN_POINT('Ctrl Pts',(172.841192559056,-54.574303158249,-42.0424115797416));
#23941=CARTESIAN_POINT('Ctrl Pts',(172.920596279528,-54.5111710705365,-41.908178056654));
#23942=CARTESIAN_POINT('Ctrl Pts',(173.,-54.463528575122,-41.7686493678573));
#23943=CARTESIAN_POINT('Ctrl Pts',(173.,-54.463528575122,-41.7686493678573));
#23944=CARTESIAN_POINT('Ctrl Pts',(173.081607306855,-54.4167863893491,-41.631757380239));
#23945=CARTESIAN_POINT('Ctrl Pts',(173.163214308534,-54.3718104458914,-41.494261598015));
#23946=CARTESIAN_POINT('Ctrl Pts',(173.244210958463,-54.3283763940785,-41.3556986057596));
#23947=CARTESIAN_POINT('Origin',(125.8,-56.3562342901464,-41.1223792414288));
#23948=CARTESIAN_POINT('',(173.,-58.153393661244,-42.));
#23949=CARTESIAN_POINT('Ctrl Pts',(174.499999999851,-58.3461592103039,-41.3228756557013));
#23950=CARTESIAN_POINT('Ctrl Pts',(174.461424720572,-58.3417521272735,-41.3666159110033));
#23951=CARTESIAN_POINT('Ctrl Pts',(174.420873583764,-58.3360427437949,-41.4087347797137));
#23952=CARTESIAN_POINT('Ctrl Pts',(174.256201391015,-58.3101344177017,-41.5653968322566));
#23953=CARTESIAN_POINT('Ctrl Pts',(174.118673603566,-58.2827371839977,-41.6665038929614));
#23954=CARTESIAN_POINT('Ctrl Pts',(173.822610223296,-58.2285507903109,-41.8308404000116));
#23955=CARTESIAN_POINT('Ctrl Pts',(173.663743266442,-58.2018772085049,-41.8942257523251));
#23956=CARTESIAN_POINT('Ctrl Pts',(173.335981739516,-58.164172163974,-41.9788285866254));
#23957=CARTESIAN_POINT('Ctrl Pts',(173.167046229782,-58.1533936609661,-42.));
#23958=CARTESIAN_POINT('Ctrl Pts',(173.,-58.1533936609661,-42.));
#23959=CARTESIAN_POINT('',(160.,-58.153393661244,-42.));
#23960=CARTESIAN_POINT('',(125.8,-58.153393661244,-42.));
#23961=CARTESIAN_POINT('',(162.,-55.5753783097334,-42.9636461796681));
#23962=CARTESIAN_POINT('Ctrl Pts',(160.,-58.1533936622468,-41.9999999973774));
#23963=CARTESIAN_POINT('Ctrl Pts',(160.022635178212,-58.1533936622468,-41.9999999973774));
#23964=CARTESIAN_POINT('Ctrl Pts',(160.045231132923,-58.151516657946,-42.0038756670436));
#23965=CARTESIAN_POINT('Ctrl Pts',(160.096465139443,-58.1432332860682,-42.0205631325354));
#23966=CARTESIAN_POINT('Ctrl Pts',(160.126719309599,-58.1360093928662,-42.0350714541553));
#23967=CARTESIAN_POINT('Ctrl Pts',(160.22848683334,-58.1032750521955,-42.0970139060601));
#23968=CARTESIAN_POINT('Ctrl Pts',(160.306498809967,-58.069336621093,-42.15765241691));
#23969=CARTESIAN_POINT('Ctrl Pts',(160.605864004126,-57.9112848828316,-42.3968423684444));
#23970=CARTESIAN_POINT('Ctrl Pts',(160.90925083337,-57.7038897039527,-42.6497063660358));
#23971=CARTESIAN_POINT('Ctrl Pts',(161.417356253422,-57.1425466698487,-42.9804088994022));
#23972=CARTESIAN_POINT('Ctrl Pts',(161.590327339247,-56.8907533740651,-43.0674615146063));
#23973=CARTESIAN_POINT('Ctrl Pts',(161.824128439415,-56.4279006785006,-43.1315274209591));
#23974=CARTESIAN_POINT('Ctrl Pts',(161.904779002332,-56.2130118801458,-43.129561872258));
#23975=CARTESIAN_POINT('Ctrl Pts',(161.983794647709,-55.8514686747774,-43.0631018472003));
#23976=CARTESIAN_POINT('Ctrl Pts',(162.,-55.7108001207802,-43.0210767068981));
#23977=CARTESIAN_POINT('Ctrl Pts',(162.,-55.5753783097334,-42.9636461796681));
#23978=CARTESIAN_POINT('',(162.,-54.463528575122,-41.7686493678573));
#23979=CARTESIAN_POINT('Origin',(162.,-56.3562342901464,-41.1223792414288));
#23980=CARTESIAN_POINT('',(125.8,-54.463528575122,-41.7686493678573));
#23981=CARTESIAN_POINT('Ctrl Pts',(172.669987974283,-54.6177973391178,42.1112356350969));
#23982=CARTESIAN_POINT('Ctrl Pts',(172.69185108023,-54.6276652871456,42.1285837612678));
#23983=CARTESIAN_POINT('Ctrl Pts',(172.73830709009,-54.644963812684,42.1577290355036));
#23984=CARTESIAN_POINT('Ctrl Pts',(172.759754438233,-54.6508063297863,42.1671363033964));
#23985=CARTESIAN_POINT('Ctrl Pts',(172.762221454692,-54.6515169577276,42.1682945422782));
#23986=CARTESIAN_POINT('Ctrl Pts',(172.894327709765,-54.5345306308711,41.8799969243054));
#23987=CARTESIAN_POINT('Ctrl Pts',(172.901371688395,-54.5373758259908,41.8854701796426));
#23988=CARTESIAN_POINT('Ctrl Pts',(172.916128759429,-54.5422404819325,41.8945407469037));
#23989=CARTESIAN_POINT('Ctrl Pts',(172.922366122002,-54.5436871571058,41.8971924349675));
#23990=CARTESIAN_POINT('Ctrl Pts',(172.922663031267,-54.5437329784674,41.8973236981606));
#23991=CARTESIAN_POINT('Ctrl Pts',(173.118667445246,-54.4512639226244,41.6487582135139));
#23992=CARTESIAN_POINT('Ctrl Pts',(173.11089229656,-54.4470863648361,41.6423565980175));
#23993=CARTESIAN_POINT('Ctrl Pts',(173.093950428767,-54.4395171511809,41.6313524583038));
#23994=CARTESIAN_POINT('Ctrl Pts',(173.08497780577,-54.4365679844252,41.6272485665385));
#23995=CARTESIAN_POINT('Ctrl Pts',(173.083104607842,-54.4359489992072,41.6263528540431));
#23996=CARTESIAN_POINT('Ctrl Pts',(173.343007180728,-54.3679972143777,41.4175195027224));
#23997=CARTESIAN_POINT('Ctrl Pts',(173.320412904725,-54.3567969036813,41.3992430163923));
#23998=CARTESIAN_POINT('Ctrl Pts',(173.271772098106,-54.3367938204293,41.368164169704));
#23999=CARTESIAN_POINT('Ctrl Pts',(173.247589489539,-54.3294488117447,41.3573046981095));
#24000=CARTESIAN_POINT('Ctrl Pts',(173.243546184418,-54.328165019947,41.3553820099255));
#24001=CARTESIAN_POINT('',(173.343007180728,-54.3679972143777,41.4175195027224));
#24002=CARTESIAN_POINT('',(172.669987974283,-54.6177973391178,42.1112356350969));
#24003=CARTESIAN_POINT('Ctrl Pts',(173.343007180728,-54.3679972143777,41.4175195027224));
#24004=CARTESIAN_POINT('Ctrl Pts',(173.118667445246,-54.4512639226244,41.6487582135139));
#24005=CARTESIAN_POINT('Ctrl Pts',(172.894327709765,-54.5345306308711,41.8799969243054));
#24006=CARTESIAN_POINT('Ctrl Pts',(172.669987974283,-54.6177973391178,42.1112356350969));
#24007=CARTESIAN_POINT('',(173.243546184425,-54.3281650199493,41.3553820099289));
#24008=CARTESIAN_POINT('Ctrl Pts',(173.343007180728,-54.3679972143777,41.4175195027224));
#24009=CARTESIAN_POINT('Ctrl Pts',(173.320412904725,-54.3567969036813,41.3992430163923));
#24010=CARTESIAN_POINT('Ctrl Pts',(173.271772098106,-54.3367938204293,41.368164169704));
#24011=CARTESIAN_POINT('Ctrl Pts',(173.247589489539,-54.3294488117447,41.3573046981095));
#24012=CARTESIAN_POINT('Ctrl Pts',(173.243546184418,-54.328165019947,41.3553820099255));
#24013=CARTESIAN_POINT('',(172.943915700111,-54.5294555245376,41.8614299246169));
#24014=CARTESIAN_POINT('Ctrl Pts',(173.243546184418,-54.328165019947,41.3553820099255));
#24015=CARTESIAN_POINT('Ctrl Pts',(173.143669356316,-54.3952618548106,41.5240646481561));
#24016=CARTESIAN_POINT('Ctrl Pts',(173.043792528214,-54.4623586896742,41.6927472863866));
#24017=CARTESIAN_POINT('Ctrl Pts',(172.943915700112,-54.5294555245378,41.8614299246172));
#24018=CARTESIAN_POINT('',(172.762221454686,-54.6515169577261,42.1682945422757));
#24019=CARTESIAN_POINT('Ctrl Pts',(172.943915700112,-54.5294555245378,41.8614299246172));
#24020=CARTESIAN_POINT('Ctrl Pts',(172.883350951638,-54.5701426689344,41.9637181305042));
#24021=CARTESIAN_POINT('Ctrl Pts',(172.822786203165,-54.610829813331,42.0660063363912));
#24022=CARTESIAN_POINT('Ctrl Pts',(172.762221454692,-54.6515169577276,42.1682945422782));
#24023=CARTESIAN_POINT('Ctrl Pts',(172.762221454692,-54.6515169577276,42.1682945422782));
#24024=CARTESIAN_POINT('Ctrl Pts',(172.759754438233,-54.6508063297863,42.1671363033964));
#24025=CARTESIAN_POINT('Ctrl Pts',(172.73830709009,-54.644963812684,42.1577290355036));
#24026=CARTESIAN_POINT('Ctrl Pts',(172.69185108023,-54.6276652871456,42.1285837612678));
#24027=CARTESIAN_POINT('Ctrl Pts',(172.669987974283,-54.6177973391178,42.1112356350969));
#24028=CARTESIAN_POINT('Ctrl Pts',(172.682265412035,-54.6233661468611,42.1209622364707));
#24029=CARTESIAN_POINT('Ctrl Pts',(172.678173128254,-54.6215008409364,42.1177253205304));
#24030=CARTESIAN_POINT('Ctrl Pts',(172.67408062253,-54.6196445624853,42.1144831049818));
#24031=CARTESIAN_POINT('Ctrl Pts',(172.669987974283,-54.6177973391178,42.1112356350969));
#24032=CARTESIAN_POINT('Ctrl Pts',(172.906556234659,-54.5402587819729,41.8897513600897));
#24033=CARTESIAN_POINT('Ctrl Pts',(172.902480958804,-54.5383400352597,41.8865042914994));
#24034=CARTESIAN_POINT('Ctrl Pts',(172.89840475748,-54.5364306414273,41.8832527979434));
#24035=CARTESIAN_POINT('Ctrl Pts',(172.894327709765,-54.5345306308711,41.8799969243054));
#24036=CARTESIAN_POINT('Ctrl Pts',(173.130847057282,-54.4571514170847,41.6585404837086));
#24037=CARTESIAN_POINT('Ctrl Pts',(173.126788789354,-54.455179229583,41.6552832624683));
#24038=CARTESIAN_POINT('Ctrl Pts',(173.12272889243,-54.4532167203693,41.6520224909049));
#24039=CARTESIAN_POINT('Ctrl Pts',(173.118667445246,-54.4512639226244,41.6487582135139));
#24040=CARTESIAN_POINT('Ctrl Pts',(173.355137879905,-54.3740440521965,41.4273296073276));
#24041=CARTESIAN_POINT('Ctrl Pts',(173.351096619904,-54.3720184239062,41.4240622334373));
#24042=CARTESIAN_POINT('Ctrl Pts',(173.34705302738,-54.3700027993113,41.4207921838665));
#24043=CARTESIAN_POINT('Ctrl Pts',(173.343007180728,-54.3679972143777,41.4175195027224));
#24044=CARTESIAN_POINT('',(172.682265412035,-54.6233661468611,42.1209622364707));
#24045=CARTESIAN_POINT('Ctrl Pts',(172.669987974283,-54.6177973391178,42.1112356350969));
#24046=CARTESIAN_POINT('Ctrl Pts',(172.673021360544,-54.6191664628845,42.1136425926307));
#24047=CARTESIAN_POINT('Ctrl Pts',(172.676054668529,-54.6205405610396,42.1160466637328));
#24048=CARTESIAN_POINT('Ctrl Pts',(172.680147061872,-54.6224011921202,42.119286319929));
#24049=CARTESIAN_POINT('Ctrl Pts',(172.681206244385,-54.6228833671227,42.1201244557024));
#24050=CARTESIAN_POINT('Ctrl Pts',(172.682265412038,-54.6233661468624,42.1209622364729));
#24051=CARTESIAN_POINT('',(173.355137879905,-54.3740440521965,41.4273296073276));
#24052=CARTESIAN_POINT('Ctrl Pts',(173.355137879905,-54.3740440521965,41.4273296073276));
#24053=CARTESIAN_POINT('Ctrl Pts',(173.130847057282,-54.4571514170847,41.6585404837086));
#24054=CARTESIAN_POINT('Ctrl Pts',(172.906556234659,-54.5402587819729,41.8897513600897));
#24055=CARTESIAN_POINT('Ctrl Pts',(172.682265412035,-54.6233661468611,42.1209622364707));
#24056=CARTESIAN_POINT('Ctrl Pts',(173.355137879905,-54.3740440521965,41.4273296073277));
#24057=CARTESIAN_POINT('Ctrl Pts',(173.354091918257,-54.3735197777119,41.4264839434067));
#24058=CARTESIAN_POINT('Ctrl Pts',(173.353045800347,-54.3729961733496,41.4256381002379));
#24059=CARTESIAN_POINT('Ctrl Pts',(173.349003338184,-54.3709757257882,41.4223693442523));
#24060=CARTESIAN_POINT('Ctrl Pts',(173.346005878614,-54.3694837124628,41.4199451463202));
#24061=CARTESIAN_POINT('Ctrl Pts',(173.343007180728,-54.3679972143777,41.4175195027224));
#24062=CARTESIAN_POINT('Ctrl Pts',(174.5,-56.8425310374202,43.0623574561495));
#24063=CARTESIAN_POINT('Ctrl Pts',(174.5,-56.7847063150805,43.076852451079));
#24064=CARTESIAN_POINT('Ctrl Pts',(174.496496807675,-56.726424924067,43.0887347398924));
#24065=CARTESIAN_POINT('Ctrl Pts',(174.472374635079,-56.5277343616924,43.1200003168992));
#24066=CARTESIAN_POINT('Ctrl Pts',(174.435819579446,-56.3890515008375,43.1269934025858));
#24067=CARTESIAN_POINT('Ctrl Pts',(174.312313762606,-56.0795034004758,43.1104492732835));
#24068=CARTESIAN_POINT('Ctrl Pts',(174.217660640189,-55.9131275752079,43.079676621033));
#24069=CARTESIAN_POINT('Ctrl Pts',(173.942183918571,-55.532355907991,42.959817332661));
#24070=CARTESIAN_POINT('Ctrl Pts',(173.741291684645,-55.3264070661798,42.8511994836494));
#24071=CARTESIAN_POINT('Ctrl Pts',(173.265184684464,-54.9358232466634,42.5556672491669));
#24072=CARTESIAN_POINT('Ctrl Pts',(172.974300346141,-54.7564787367862,42.3519561225039));
#24073=CARTESIAN_POINT('Ctrl Pts',(172.682265412035,-54.6233661468611,42.1209622364707));
#24074=CARTESIAN_POINT('Ctrl Pts',(174.666585068858,-56.8020063133375,42.9006926242979));
#24075=CARTESIAN_POINT('Ctrl Pts',(174.666275223311,-56.7442298071472,42.9151773304318));
#24076=CARTESIAN_POINT('Ctrl Pts',(174.662752482402,-56.6858660630933,42.9267775056715));
#24077=CARTESIAN_POINT('Ctrl Pts',(174.639550570743,-56.4864395729044,42.9561400122007));
#24078=CARTESIAN_POINT('Ctrl Pts',(174.605246474233,-56.3464817138786,42.9602032167489));
#24079=CARTESIAN_POINT('Ctrl Pts',(174.48920343284,-56.0328192806896,42.9343985844122));
#24080=CARTESIAN_POINT('Ctrl Pts',(174.400067029284,-55.8634208915866,42.8969672866207));
#24081=CARTESIAN_POINT('Ctrl Pts',(174.138352490568,-55.4746412639251,42.7605554030612));
#24082=CARTESIAN_POINT('Ctrl Pts',(173.945647760261,-55.2634045021095,42.6421788065363));
#24083=CARTESIAN_POINT('Ctrl Pts',(173.483301232679,-54.8620390670757,42.3305939920553));
#24084=CARTESIAN_POINT('Ctrl Pts',(173.197434721993,-54.6771744507838,42.1213898659891));
#24085=CARTESIAN_POINT('Ctrl Pts',(172.906556234659,-54.5402587819729,41.8897513600897));
#24086=CARTESIAN_POINT('Ctrl Pts',(174.833170137715,-56.7614815892548,42.7390277924464));
#24087=CARTESIAN_POINT('Ctrl Pts',(174.832550305402,-56.7037516530913,42.7534976988416));
#24088=CARTESIAN_POINT('Ctrl Pts',(174.829009502811,-56.645308594404,42.7648244865385));
#24089=CARTESIAN_POINT('Ctrl Pts',(174.806721608943,-56.4451411607773,42.7922706501334));
#24090=CARTESIAN_POINT('Ctrl Pts',(174.774691045787,-56.303909416709,42.7933951250364));
#24091=CARTESIAN_POINT('Ctrl Pts',(174.666060639652,-55.9861389428714,42.7583804524309));
#24092=CARTESIAN_POINT('Ctrl Pts',(174.58251031073,-55.8137112952995,42.7142096468544));
#24093=CARTESIAN_POINT('Ctrl Pts',(174.334441347141,-55.4169347605697,42.561393695158));
#24094=CARTESIAN_POINT('Ctrl Pts',(174.149980589901,-55.2004048120655,42.4331810744332));
#24095=CARTESIAN_POINT('Ctrl Pts',(173.701401705862,-54.7882591897525,42.1055501983502));
#24096=CARTESIAN_POINT('Ctrl Pts',(173.420397262025,-54.5979019067952,41.8910633003636));
#24097=CARTESIAN_POINT('Ctrl Pts',(173.130847057282,-54.4571514170847,41.6585404837086));
#24098=CARTESIAN_POINT('Ctrl Pts',(174.999755206573,-56.7209568651721,42.5773629605948));
#24099=CARTESIAN_POINT('Ctrl Pts',(174.998825528713,-56.663275145158,42.5918225781943));
#24100=CARTESIAN_POINT('Ctrl Pts',(174.995265177538,-56.6047497334302,42.6028672523175));
#24101=CARTESIAN_POINT('Ctrl Pts',(174.973897544607,-56.4038463719893,42.6284103454349));
#24102=CARTESIAN_POINT('Ctrl Pts',(174.944117940575,-56.2613396297502,42.6266049391994));
#24103=CARTESIAN_POINT('Ctrl Pts',(174.842950309886,-55.9394548230851,42.5823297635595));
#24104=CARTESIAN_POINT('Ctrl Pts',(174.764916699824,-55.7640046116782,42.5315003124422));
#24105=CARTESIAN_POINT('Ctrl Pts',(174.530609919138,-55.3592201165037,42.3621317655582));
#24106=CARTESIAN_POINT('Ctrl Pts',(174.354336665516,-55.1374022479952,42.2241603973201));
#24107=CARTESIAN_POINT('Ctrl Pts',(173.919518254077,-54.7144750101649,41.8804769412387));
#24108=CARTESIAN_POINT('Ctrl Pts',(173.643531637876,-54.5185976207928,41.6604970438488));
#24109=CARTESIAN_POINT('Ctrl Pts',(173.355137879905,-54.3740440521965,41.4273296073276));
#24110=CARTESIAN_POINT('',(174.5,-56.8425310374202,43.0623574561495));
#24111=CARTESIAN_POINT('Ctrl Pts',(172.682265412035,-54.6233661468611,42.1209622364707));
#24112=CARTESIAN_POINT('Ctrl Pts',(172.974300346141,-54.7564787367862,42.3519561225039));
#24113=CARTESIAN_POINT('Ctrl Pts',(173.265184684464,-54.9358232466634,42.5556672491669));
#24114=CARTESIAN_POINT('Ctrl Pts',(173.741291684645,-55.3264070661798,42.8511994836494));
#24115=CARTESIAN_POINT('Ctrl Pts',(173.942183918571,-55.532355907991,42.959817332661));
#24116=CARTESIAN_POINT('Ctrl Pts',(174.217660640189,-55.9131275752079,43.079676621033));
#24117=CARTESIAN_POINT('Ctrl Pts',(174.312313762606,-56.0795034004758,43.1104492732835));
#24118=CARTESIAN_POINT('Ctrl Pts',(174.435819579446,-56.3890515008375,43.1269934025858));
#24119=CARTESIAN_POINT('Ctrl Pts',(174.472374635079,-56.5277343616924,43.1200003168992));
#24120=CARTESIAN_POINT('Ctrl Pts',(174.496496807675,-56.726424924067,43.0887347398924));
#24121=CARTESIAN_POINT('Ctrl Pts',(174.5,-56.7847063150805,43.076852451079));
#24122=CARTESIAN_POINT('Ctrl Pts',(174.5,-56.8425310374202,43.0623574561495));
#24123=CARTESIAN_POINT('',(174.999755206573,-56.7209568651721,42.5773629605948));
#24124=CARTESIAN_POINT('',(174.5,-56.8425310374202,43.0623574561495));
#24125=CARTESIAN_POINT('Ctrl Pts',(174.999755206573,-56.7209568651721,42.5773629605948));
#24126=CARTESIAN_POINT('Ctrl Pts',(174.998825528713,-56.663275145158,42.5918225781943));
#24127=CARTESIAN_POINT('Ctrl Pts',(174.995265177538,-56.6047497334302,42.6028672523175));
#24128=CARTESIAN_POINT('Ctrl Pts',(174.973897544607,-56.4038463719893,42.6284103454349));
#24129=CARTESIAN_POINT('Ctrl Pts',(174.944117940575,-56.2613396297502,42.6266049391994));
#24130=CARTESIAN_POINT('Ctrl Pts',(174.842950309886,-55.9394548230851,42.5823297635595));
#24131=CARTESIAN_POINT('Ctrl Pts',(174.764916699824,-55.7640046116782,42.5315003124422));
#24132=CARTESIAN_POINT('Ctrl Pts',(174.530609919138,-55.3592201165037,42.3621317655582));
#24133=CARTESIAN_POINT('Ctrl Pts',(174.354336665516,-55.1374022479952,42.2241603973201));
#24134=CARTESIAN_POINT('Ctrl Pts',(173.919518254077,-54.7144750101649,41.8804769412387));
#24135=CARTESIAN_POINT('Ctrl Pts',(173.643531637876,-54.5185976207928,41.6604970438488));
#24136=CARTESIAN_POINT('Ctrl Pts',(173.355137879905,-54.3740440521965,41.4273296073276));
#24137=CARTESIAN_POINT('Origin',(174.75,-56.3562342901464,41.1223792414288));
#24138=CARTESIAN_POINT('',(175.,-56.7512686935136,42.5694272088978));
#24139=CARTESIAN_POINT('',(174.5,-56.8829468279694,43.0517765313875));
#24140=CARTESIAN_POINT('',(175.,-56.7512686935136,42.5694272088978));
#24141=CARTESIAN_POINT('',(174.499999999905,-58.3461592102992,41.3228756557482));
#24142=CARTESIAN_POINT('Origin',(174.5,-56.3562342901464,41.1223792414288));
#24143=CARTESIAN_POINT('',(175.,-57.351354804662,40.));
#24144=CARTESIAN_POINT('Ctrl Pts',(175.,-57.351354804662,40.));
#24145=CARTESIAN_POINT('Ctrl Pts',(175.,-57.4269240433685,40.0670009716211));
#24146=CARTESIAN_POINT('Ctrl Pts',(174.996519917819,-57.4970226095956,40.1383691282534));
#24147=CARTESIAN_POINT('Ctrl Pts',(174.978867869175,-57.6455132484847,40.3052809972307));
#24148=CARTESIAN_POINT('Ctrl Pts',(174.957119187857,-57.7379468702121,40.4252008690902));
#24149=CARTESIAN_POINT('Ctrl Pts',(174.904968042358,-57.87254986344,40.6161672831003));
#24150=CARTESIAN_POINT('Ctrl Pts',(174.86686770893,-57.9430044328017,40.7239686970479));
#24151=CARTESIAN_POINT('Ctrl Pts',(174.776779134635,-58.0729443622281,40.9266860356746));
#24152=CARTESIAN_POINT('Ctrl Pts',(174.701138126955,-58.1568455611626,41.0593011894553));
#24153=CARTESIAN_POINT('Ctrl Pts',(174.588496139891,-58.2661562974069,41.217054380861));
#24154=CARTESIAN_POINT('Ctrl Pts',(174.545769052472,-58.3053873720851,41.270978428147));
#24155=CARTESIAN_POINT('Ctrl Pts',(174.499999999896,-58.3461592104135,41.3228756556501));
#24156=CARTESIAN_POINT('Origin',(175.,-56.3562342901464,41.1223792414288));
#24157=CARTESIAN_POINT('Ctrl Pts',(174.5,-56.8829468279694,43.0517765313875));
#24158=CARTESIAN_POINT('Ctrl Pts',(174.5,-56.8695122257409,43.0554440878163));
#24159=CARTESIAN_POINT('Ctrl Pts',(174.5,-56.8560393157734,43.0589713192462));
#24160=CARTESIAN_POINT('Ctrl Pts',(174.5,-56.8425310374202,43.0623574561495));
#24161=CARTESIAN_POINT('Ctrl Pts',(174.666666666667,-56.8390541164841,42.890993423891));
#24162=CARTESIAN_POINT('Ctrl Pts',(174.666666666667,-56.8267390644414,42.8943553506173));
#24163=CARTESIAN_POINT('Ctrl Pts',(174.666639498249,-56.8143888954835,42.8975886395879));
#24164=CARTESIAN_POINT('Ctrl Pts',(174.666585068858,-56.8020063133375,42.9006926242979));
#24165=CARTESIAN_POINT('Ctrl Pts',(174.833333333333,-56.7951614049989,42.7302103163944));
#24166=CARTESIAN_POINT('Ctrl Pts',(174.833333333333,-56.7839659031418,42.7332666134184));
#24167=CARTESIAN_POINT('Ctrl Pts',(174.833278996499,-56.7727384751935,42.7362059599296));
#24168=CARTESIAN_POINT('Ctrl Pts',(174.833170137715,-56.7614815892548,42.7390277924464));
#24169=CARTESIAN_POINT('Ctrl Pts',(175.,-56.7512686935137,42.5694272088978));
#24170=CARTESIAN_POINT('Ctrl Pts',(175.,-56.7411927418423,42.5721778762194));
#24171=CARTESIAN_POINT('Ctrl Pts',(174.999918494748,-56.7310880549036,42.5748232802713));
#24172=CARTESIAN_POINT('Ctrl Pts',(174.999755206573,-56.7209568651721,42.5773629605948));
#24173=CARTESIAN_POINT('Ctrl Pts',(175.,-56.7512686935137,42.5694272088978));
#24174=CARTESIAN_POINT('Ctrl Pts',(175.,-56.7411927418423,42.5721778762194));
#24175=CARTESIAN_POINT('Ctrl Pts',(174.999918494748,-56.7310880549036,42.5748232802713));
#24176=CARTESIAN_POINT('Ctrl Pts',(174.999755206573,-56.7209568651721,42.5773629605948));
#24177=CARTESIAN_POINT('Ctrl Pts',(174.5,-56.8425310374202,43.0623574561495));
#24178=CARTESIAN_POINT('Ctrl Pts',(174.5,-56.8560393157734,43.0589713192462));
#24179=CARTESIAN_POINT('Ctrl Pts',(174.5,-56.8695122257409,43.0554440878163));
#24180=CARTESIAN_POINT('Ctrl Pts',(174.5,-56.8829468279694,43.0517765313875));
#24181=CARTESIAN_POINT('Ctrl Pts',(173.243546184425,-54.3281650199493,41.3553820099289));
#24182=CARTESIAN_POINT('Ctrl Pts',(173.162767797901,-54.3716994765092,41.4940379614493));
#24183=CARTESIAN_POINT('Ctrl Pts',(173.081384049463,-54.41674640089,41.6316402676231));
#24184=CARTESIAN_POINT('Ctrl Pts',(173.,-54.463528575122,41.7686493678573));
#24185=CARTESIAN_POINT('Ctrl Pts',(173.083104607845,-54.4359489992082,41.6263528540445));
#24186=CARTESIAN_POINT('Ctrl Pts',(173.055672188531,-54.4392567683325,41.676877439586));
#24187=CARTESIAN_POINT('Ctrl Pts',(173.027836194607,-54.4482298591699,41.7238446245605));
#24188=CARTESIAN_POINT('Ctrl Pts',(173.,-54.463528575122,41.7686493678573));
#24189=CARTESIAN_POINT('Ctrl Pts',(172.922663031266,-54.5437329784671,41.8973236981601));
#24190=CARTESIAN_POINT('Ctrl Pts',(172.948576579161,-54.5068140601558,41.8597169177226));
#24191=CARTESIAN_POINT('Ctrl Pts',(172.974288339751,-54.4797133174499,41.8160489814978));
#24192=CARTESIAN_POINT('Ctrl Pts',(173.,-54.463528575122,41.7686493678573));
#24193=CARTESIAN_POINT('Ctrl Pts',(172.762221454686,-54.6515169577261,42.1682945422757));
#24194=CARTESIAN_POINT('Ctrl Pts',(172.841480969791,-54.5743713519791,42.0425563958593));
#24195=CARTESIAN_POINT('Ctrl Pts',(172.920740484895,-54.5111967757298,41.9082533384352));
#24196=CARTESIAN_POINT('Ctrl Pts',(173.,-54.463528575122,41.7686493678573));
#24197=CARTESIAN_POINT('',(173.,-54.463528575122,41.7686493678573));
#24198=CARTESIAN_POINT('Ctrl Pts',(173.243546184425,-54.3281650199493,41.3553820099289));
#24199=CARTESIAN_POINT('Ctrl Pts',(173.162767797901,-54.3716994765092,41.4940379614493));
#24200=CARTESIAN_POINT('Ctrl Pts',(173.081384049463,-54.41674640089,41.6316402676231));
#24201=CARTESIAN_POINT('Ctrl Pts',(173.,-54.463528575122,41.7686493678573));
#24202=CARTESIAN_POINT('Ctrl Pts',(173.,-54.463528575122,41.7686493678573));
#24203=CARTESIAN_POINT('Ctrl Pts',(172.920740484895,-54.5111967757298,41.9082533384352));
#24204=CARTESIAN_POINT('Ctrl Pts',(172.841480969791,-54.5743713519791,42.0425563958593));
#24205=CARTESIAN_POINT('Ctrl Pts',(172.762221454686,-54.6515169577261,42.1682945422757));
#24206=CARTESIAN_POINT('Origin',(173.,-45.,45.));
#24207=CARTESIAN_POINT('',(175.,-41.1096563890154,56.3518820725231));
#24208=CARTESIAN_POINT('Origin',(175.,-45.,45.));
#24209=CARTESIAN_POINT('',(173.,-41.7580469908461,54.4599017271026));
#24210=CARTESIAN_POINT('Origin',(173.,-41.1096563890154,56.3518820725231));
#24211=CARTESIAN_POINT('Origin',(173.,-45.,45.));
#24212=CARTESIAN_POINT('Origin',(175.,0.,0.));
#24213=CARTESIAN_POINT('',(175.,-41.1096563890154,-56.3518820725231));
#24214=CARTESIAN_POINT('Origin',(175.,-45.,-45.));
#24215=CARTESIAN_POINT('',(175.,-32.,-58.));
#24216=CARTESIAN_POINT('Origin',(175.,-32.,-32.));
#24217=CARTESIAN_POINT('',(175.,32.,-58.));
#24218=CARTESIAN_POINT('',(175.,-16.,-58.));
#24219=CARTESIAN_POINT('',(175.,41.1096563890154,-56.3518820725231));
#24220=CARTESIAN_POINT('Origin',(175.,32.,-32.));
#24221=CARTESIAN_POINT('',(175.,56.3518820725231,-41.1096563890154));
#24222=CARTESIAN_POINT('Origin',(175.,45.,-45.));
#24223=CARTESIAN_POINT('',(175.,57.9807621135332,-31.));
#24224=CARTESIAN_POINT('Origin',(175.,32.,-32.));
#24225=CARTESIAN_POINT('',(175.,64.,-31.));
#24226=CARTESIAN_POINT('',(175.,26.5,-31.));
#24227=CARTESIAN_POINT('',(175.,64.,31.));
#24228=CARTESIAN_POINT('',(175.,64.,-16.5));
#24229=CARTESIAN_POINT('',(175.,57.9807621135332,31.));
#24230=CARTESIAN_POINT('',(175.,26.5,31.));
#24231=CARTESIAN_POINT('',(175.,56.3518820725231,41.1096563890154));
#24232=CARTESIAN_POINT('Origin',(175.,32.,32.));
#24233=CARTESIAN_POINT('',(175.,41.1096563890154,56.3518820725231));
#24234=CARTESIAN_POINT('Origin',(175.,45.,45.));
#24235=CARTESIAN_POINT('',(175.,32.,58.));
#24236=CARTESIAN_POINT('Origin',(175.,32.,32.));
#24237=CARTESIAN_POINT('',(175.,-32.,58.));
#24238=CARTESIAN_POINT('',(175.,16.,58.));
#24239=CARTESIAN_POINT('Origin',(175.,-32.,32.));
#24240=CARTESIAN_POINT('',(175.,-30.,40.));
#24241=CARTESIAN_POINT('',(175.,-30.,-40.));
#24242=CARTESIAN_POINT('Origin',(138.1,65.75,25.4));
#24243=CARTESIAN_POINT('',(132.55,66.,25.4));
#24244=CARTESIAN_POINT('Origin',(138.1,66.,25.4));
#24245=CARTESIAN_POINT('',(133.05,65.5,25.4));
#24246=CARTESIAN_POINT('',(132.8,65.75,25.4));
#24247=CARTESIAN_POINT('Origin',(138.1,65.5,25.4));
#24248=CARTESIAN_POINT('Origin',(175.,66.,-33.));
#24249=CARTESIAN_POINT('',(127.8,66.,31.));
#24250=CARTESIAN_POINT('',(127.8,66.,-31.));
#24251=CARTESIAN_POINT('',(127.8,66.,-16.5));
#24252=CARTESIAN_POINT('',(173.,66.,31.));
#24253=CARTESIAN_POINT('',(162.7,66.,31.));
#24254=CARTESIAN_POINT('',(173.,66.,-31.));
#24255=CARTESIAN_POINT('',(173.,66.,-16.5));
#24256=CARTESIAN_POINT('',(162.7,66.,-31.));
#24257=CARTESIAN_POINT('',(156.35,66.,-25.4));
#24258=CARTESIAN_POINT('Origin',(161.9,66.,-25.4));
#24259=CARTESIAN_POINT('',(132.55,66.,-25.4));
#24260=CARTESIAN_POINT('Origin',(138.1,66.,-25.4));
#24261=CARTESIAN_POINT('',(140.,66.,1.22464679914735E-15));
#24262=CARTESIAN_POINT('Origin',(150.,66.,0.));
#24263=CARTESIAN_POINT('',(156.35,66.,25.4));
#24264=CARTESIAN_POINT('Origin',(161.9,66.,25.4));
#24265=CARTESIAN_POINT('Origin',(138.1,66.,25.4));
#24266=CARTESIAN_POINT('',(133.05,49.,25.4));
#24267=CARTESIAN_POINT('',(133.05,66.,25.4));
#24268=CARTESIAN_POINT('Origin',(138.1,49.,25.4));
#24269=CARTESIAN_POINT('Origin',(161.9,65.75,-25.4));
#24270=CARTESIAN_POINT('',(156.85,65.5,-25.4));
#24271=CARTESIAN_POINT('',(156.6,65.75,-25.4));
#24272=CARTESIAN_POINT('Origin',(161.9,65.5,-25.4));
#24273=CARTESIAN_POINT('Origin',(161.9,66.,-25.4));
#24274=CARTESIAN_POINT('',(156.85,49.,-25.4));
#24275=CARTESIAN_POINT('',(156.85,66.,-25.4));
#24276=CARTESIAN_POINT('Origin',(161.9,49.,-25.4));
#24277=CARTESIAN_POINT('Origin',(161.9,65.75,25.4));
#24278=CARTESIAN_POINT('',(156.85,65.5,25.4));
#24279=CARTESIAN_POINT('',(156.6,65.75,25.4));
#24280=CARTESIAN_POINT('Origin',(161.9,65.5,25.4));
#24281=CARTESIAN_POINT('Origin',(161.9,66.,25.4));
#24282=CARTESIAN_POINT('',(156.85,49.,25.4));
#24283=CARTESIAN_POINT('',(156.85,66.,25.4));
#24284=CARTESIAN_POINT('Origin',(161.9,49.,25.4));
#24285=CARTESIAN_POINT('Origin',(138.1,65.75,-25.4));
#24286=CARTESIAN_POINT('',(133.05,65.5,-25.4));
#24287=CARTESIAN_POINT('',(132.8,65.75,-25.4));
#24288=CARTESIAN_POINT('Origin',(138.1,65.5,-25.4));
#24289=CARTESIAN_POINT('Origin',(138.1,66.,-25.4));
#24290=CARTESIAN_POINT('',(133.05,49.,-25.4));
#24291=CARTESIAN_POINT('',(133.05,66.,-25.4));
#24292=CARTESIAN_POINT('Origin',(138.1,49.,-25.4));
#24293=CARTESIAN_POINT('Origin',(150.,65.75,0.));
#24294=CARTESIAN_POINT('',(140.5,65.5,-1.16341445918998E-15));
#24295=CARTESIAN_POINT('',(140.25,65.75,1.19403062916867E-15));
#24296=CARTESIAN_POINT('Origin',(150.,65.5,0.));
#24297=CARTESIAN_POINT('Origin',(150.,66.,0.));
#24298=CARTESIAN_POINT('',(140.5024163973,35.9970291210556,0.000659424480330972));
#24299=CARTESIAN_POINT('',(140.5,66.,-1.16341445918998E-15));
#24300=CARTESIAN_POINT('',(140.502173012404,20.0025228153278,0.000820030757110642));
#24301=CARTESIAN_POINT('Ctrl Pts',(140.502472449209,20.002870454282,0.000933029370863217));
#24302=CARTESIAN_POINT('Ctrl Pts',(140.502079425243,20.0023872760223,-0.513648430176057));
#24303=CARTESIAN_POINT('Ctrl Pts',(140.580570085935,20.1416700372709,-1.54333997704372));
#24304=CARTESIAN_POINT('Ctrl Pts',(140.940135198509,20.7760302225561,-2.96372789758379));
#24305=CARTESIAN_POINT('Ctrl Pts',(141.613773440736,22.0590093116005,-4.60669302069982));
#24306=CARTESIAN_POINT('Ctrl Pts',(142.51650955026,24.0303305797403,-5.90697582915808));
#24307=CARTESIAN_POINT('Ctrl Pts',(143.197512601211,26.7250000406644,-6.63359194555753));
#24308=CARTESIAN_POINT('Ctrl Pts',(143.198827571655,29.2764783425835,-6.63422718178349));
#24309=CARTESIAN_POINT('Ctrl Pts',(142.61406517216,31.5865966550244,-6.01113699999118));
#24310=CARTESIAN_POINT('Ctrl Pts',(141.828024497579,33.5000354399014,-4.9254108406999));
#24311=CARTESIAN_POINT('Ctrl Pts',(141.077842938275,34.9766629596617,-3.42496442652058));
#24312=CARTESIAN_POINT('Ctrl Pts',(140.593484092959,35.8349779276441,-1.71480123653937));
#24313=CARTESIAN_POINT('Ctrl Pts',(140.502479291261,35.9969413163685,-0.513694213206118));
#24314=CARTESIAN_POINT('Ctrl Pts',(140.502956649271,35.9963648994868,0.00080685693081263));
#24315=CARTESIAN_POINT('Origin',(150.,20.,0.));
#24316=CARTESIAN_POINT('',(143.175401713146,28.,6.60869565217391));
#24317=CARTESIAN_POINT('Ctrl Pts',(143.175401713146,28.,6.60869565217391));
#24318=CARTESIAN_POINT('Ctrl Pts',(143.175401713146,27.3777956850962,6.60869565217391));
#24319=CARTESIAN_POINT('Ctrl Pts',(143.05419832612,26.1354767285296,6.48707115577184));
#24320=CARTESIAN_POINT('Ctrl Pts',(142.44802175351,23.8795076799284,5.80658697436831));
#24321=CARTESIAN_POINT('Ctrl Pts',(141.407577159842,21.6081542657929,4.31108301914421));
#24322=CARTESIAN_POINT('Ctrl Pts',(140.622943710823,20.2151487945374,2.05828551505037));
#24323=CARTESIAN_POINT('Ctrl Pts',(140.502865436407,20.0033535873405,0.515466350059816));
#24324=CARTESIAN_POINT('Ctrl Pts',(140.502472449209,20.002870454282,0.000933029370863217));
#24325=CARTESIAN_POINT('Ctrl Pts',(140.502956649271,35.9963648994868,0.00080685693081263));
#24326=CARTESIAN_POINT('Ctrl Pts',(140.503434038327,35.9957884451177,0.515341387647046));
#24327=CARTESIAN_POINT('Ctrl Pts',(140.623315085809,35.7840723365628,2.05816288432255));
#24328=CARTESIAN_POINT('Ctrl Pts',(141.409078045969,34.3900535537995,4.31115068270884));
#24329=CARTESIAN_POINT('Ctrl Pts',(142.448051488086,32.1203379370536,5.80658533410845));
#24330=CARTESIAN_POINT('Ctrl Pts',(143.054377037915,29.8642777153372,6.48707561474873));
#24331=CARTESIAN_POINT('Ctrl Pts',(143.175401713146,28.622204314904,6.60869565217392));
#24332=CARTESIAN_POINT('Ctrl Pts',(143.175401713146,28.,6.60869565217392));
#24333=CARTESIAN_POINT('Ctrl Pts',(141.738644179071,28.,6.));
#24334=CARTESIAN_POINT('Ctrl Pts',(141.738644179071,28.466653236178,6.));
#24335=CARTESIAN_POINT('Ctrl Pts',(141.592140624844,29.3982082865029,5.88958180812713));
#24336=CARTESIAN_POINT('Ctrl Pts',(140.858167590841,31.0902534527902,5.27176826386162));
#24337=CARTESIAN_POINT('Ctrl Pts',(139.600462897751,32.7925401653496,3.9140710145646));
#24338=CARTESIAN_POINT('Ctrl Pts',(138.45904623122,34.0471489107534,1.45951606005547));
#24339=CARTESIAN_POINT('Ctrl Pts',(138.453250392708,34.0518051367242,-1.13339199495755));
#24340=CARTESIAN_POINT('Ctrl Pts',(139.199494083175,33.2324972197463,-3.10950717670948));
#24341=CARTESIAN_POINT('Ctrl Pts',(140.107608602332,32.125026579926,-4.4717545790565));
#24342=CARTESIAN_POINT('Ctrl Pts',(141.059131524193,30.6899474912683,-5.45747964472883));
#24343=CARTESIAN_POINT('Ctrl Pts',(141.767001797266,28.9573587569376,-6.02317994135606));
#24344=CARTESIAN_POINT('Ctrl Pts',(141.76540999094,27.0437500304983,-6.02260321372987));
#24345=CARTESIAN_POINT('Ctrl Pts',(140.941037876631,25.0227479348052,-5.36291226594614));
#24346=CARTESIAN_POINT('Ctrl Pts',(139.848252059838,23.5442569837004,-4.18239234774062));
#24347=CARTESIAN_POINT('Ctrl Pts',(139.032795240301,22.5820226669171,-2.69075295964843));
#24348=CARTESIAN_POINT('Ctrl Pts',(138.452453581158,21.9476723726241,-0.97136281248494));
#24349=CARTESIAN_POINT('Ctrl Pts',(138.458852046436,21.9523990462047,1.45962302485803));
#24350=CARTESIAN_POINT('Ctrl Pts',(139.598646035598,23.2061156993447,3.91400958317042));
#24351=CARTESIAN_POINT('Ctrl Pts',(140.858131596355,24.9096307599463,5.27176975304492));
#24352=CARTESIAN_POINT('Ctrl Pts',(141.591924289514,26.6016075463972,5.88957775984548));
#24353=CARTESIAN_POINT('Ctrl Pts',(141.738644179071,27.533346763822,6.));
#24354=CARTESIAN_POINT('Ctrl Pts',(141.738644179071,28.,6.));
#24355=CARTESIAN_POINT('Ctrl Pts',(142.043965696508,28.,6.));
#24356=CARTESIAN_POINT('Ctrl Pts',(142.043965696508,28.489619376602,6.));
#24357=CARTESIAN_POINT('Ctrl Pts',(141.905479893413,29.4675535704741,5.87773555290971));
#24358=CARTESIAN_POINT('Ctrl Pts',(141.217720935708,31.2218964506089,5.20599667447634));
#24359=CARTESIAN_POINT('Ctrl Pts',(140.053424701285,32.9275777830355,3.7514473788431));
#24360=CARTESIAN_POINT('Ctrl Pts',(139.061090117389,34.0443918223547,1.33284727256326));
#24361=CARTESIAN_POINT('Ctrl Pts',(139.059027025196,34.0430682506412,-1.03627554436337));
#24362=CARTESIAN_POINT('Ctrl Pts',(139.702875040431,33.322365386674,-2.95193917049126));
#24363=CARTESIAN_POINT('Ctrl Pts',(140.524068736404,32.258214133341,-4.35124876313713));
#24364=CARTESIAN_POINT('Ctrl Pts',(141.404330684989,30.8114576637609,-5.40538794487833));
#24365=CARTESIAN_POINT('Ctrl Pts',(142.070230027061,29.0064483130425,-6.02585560608033));
#24366=CARTESIAN_POINT('Ctrl Pts',(142.068792362312,26.9942998217749,-6.0249220615482));
#24367=CARTESIAN_POINT('Ctrl Pts',(141.2929367632,24.8886851324338,-5.30236034708324));
#24368=CARTESIAN_POINT('Ctrl Pts',(140.285567337581,23.4147662511711,-4.04197533388614));
#24369=CARTESIAN_POINT('Ctrl Pts',(139.558150790354,22.512706151362,-2.54371757658131));
#24370=CARTESIAN_POINT('Ctrl Pts',(139.058822833885,21.957295463926,-0.888260075897155));
#24371=CARTESIAN_POINT('Ctrl Pts',(139.061067834149,21.9556534193931,1.33302010233888));
#24372=CARTESIAN_POINT('Ctrl Pts',(140.052488123096,23.0724505819996,3.75147334802102));
#24373=CARTESIAN_POINT('Ctrl Pts',(141.217701781722,24.7780427741925,5.20600221509276));
#24374=CARTESIAN_POINT('Ctrl Pts',(141.905368227135,26.5324235696485,5.87774188530814));
#24375=CARTESIAN_POINT('Ctrl Pts',(142.043965696508,27.510380623398,6.));
#24376=CARTESIAN_POINT('Ctrl Pts',(142.043965696508,28.,6.));
#24377=CARTESIAN_POINT('Ctrl Pts',(142.57788822158,28.,6.12463030305979));
#24378=CARTESIAN_POINT('Ctrl Pts',(142.57788822158,28.5395615790993,6.12463030305979));
#24379=CARTESIAN_POINT('Ctrl Pts',(142.453723397324,29.6171845933956,5.99156227883951));
#24380=CARTESIAN_POINT('Ctrl Pts',(141.846341502135,31.5440219059675,5.268772011394));
#24381=CARTESIAN_POINT('Ctrl Pts',(140.844323830014,33.4026543544232,3.71115220069704));
#24382=CARTESIAN_POINT('Ctrl Pts',(140.100655327228,34.5544656664828,1.26154906292248));
#24383=CARTESIAN_POINT('Ctrl Pts',(140.103937101032,34.5500472995073,-0.981414646809834));
#24384=CARTESIAN_POINT('Ctrl Pts',(140.578675206434,33.8115119944716,-2.89529601543811));
#24385=CARTESIAN_POINT('Ctrl Pts',(141.251976097117,32.6708724945202,-4.35505081975209));
#24386=CARTESIAN_POINT('Ctrl Pts',(142.0093534077,31.0940053129146,-5.48116085900691));
#24387=CARTESIAN_POINT('Ctrl Pts',(142.601771765176,29.1092669955987,-6.15227033925031));
#24388=CARTESIAN_POINT('Ctrl Pts',(142.600547825936,26.8912001711519,-6.15101629252184));
#24389=CARTESIAN_POINT('Ctrl Pts',(141.909317212412,24.5751011285043,-5.37058697183273));
#24390=CARTESIAN_POINT('Ctrl Pts',(141.049251669911,22.9739732545708,-4.02397204951632));
#24391=CARTESIAN_POINT('Ctrl Pts',(140.47000213459,22.0173629223548,-2.48551241031029));
#24392=CARTESIAN_POINT('Ctrl Pts',(140.104591253159,21.450847766609,-0.841472379185922));
#24393=CARTESIAN_POINT('Ctrl Pts',(140.100297492759,21.4446966445209,1.26149033180786));
#24394=CARTESIAN_POINT('Ctrl Pts',(140.844653274062,22.5980254068523,3.7109471930761));
#24395=CARTESIAN_POINT('Ctrl Pts',(141.846258982871,24.4557692411548,5.2687424407902));
#24396=CARTESIAN_POINT('Ctrl Pts',(142.453763523801,26.3828695847505,5.99154161878406));
#24397=CARTESIAN_POINT('Ctrl Pts',(142.57788822158,27.4604384209008,6.12463030305979));
#24398=CARTESIAN_POINT('Ctrl Pts',(142.57788822158,28.,6.12463030305979));
#24399=CARTESIAN_POINT('Ctrl Pts',(143.016103530135,28.,6.44419328073923));
#24400=CARTESIAN_POINT('Ctrl Pts',(143.016103530135,28.5974178246517,6.44419328073923));
#24401=CARTESIAN_POINT('Ctrl Pts',(142.896149230359,29.7901391902406,6.31763407548422));
#24402=CARTESIAN_POINT('Ctrl Pts',(142.301895316234,31.9474466700465,5.61797095740714));
#24403=CARTESIAN_POINT('Ctrl Pts',(141.303027832022,34.0939356482408,4.09471435137365));
#24404=CARTESIAN_POINT('Ctrl Pts',(140.467893969615,35.6111302989085,1.4824078247523));
#24405=CARTESIAN_POINT('Ctrl Pts',(140.466527313903,35.6142168793452,-1.15183663734545));
#24406=CARTESIAN_POINT('Ctrl Pts',(141.007809366,34.627410681629,-3.23372564469958));
#24407=CARTESIAN_POINT('Ctrl Pts',(141.70681890823,33.2513146547413,-4.72180677695984));
#24408=CARTESIAN_POINT('Ctrl Pts',(142.46286099909,31.4387556515361,-5.82640140894008));
#24409=CARTESIAN_POINT('Ctrl Pts',(143.038905695447,29.226321106751,-6.47066418005133));
#24410=CARTESIAN_POINT('Ctrl Pts',(143.037683909907,26.7748498264222,-6.46980943905863));
#24411=CARTESIAN_POINT('Ctrl Pts',(142.366284600791,24.1937858935098,-5.7192270911062));
#24412=CARTESIAN_POINT('Ctrl Pts',(141.502681958482,22.3334174658961,-4.39763660762648));
#24413=CARTESIAN_POINT('Ctrl Pts',(140.885992207105,21.1479815909271,-2.79104896834084));
#24414=CARTESIAN_POINT('Ctrl Pts',(140.466409892293,20.3855543526367,-0.987293662979608));
#24415=CARTESIAN_POINT('Ctrl Pts',(140.4678361008,20.3881444401133,1.48246616303375));
#24416=CARTESIAN_POINT('Ctrl Pts',(141.302327362314,21.9049988827169,4.09461479833817));
#24417=CARTESIAN_POINT('Ctrl Pts',(142.301871353512,24.0523749164083,5.61796148916296));
#24418=CARTESIAN_POINT('Ctrl Pts',(142.896065782025,26.2097035136665,6.3176258699495));
#24419=CARTESIAN_POINT('Ctrl Pts',(143.016103530135,27.4025821753484,6.44419328073922));
#24420=CARTESIAN_POINT('Ctrl Pts',(143.016103530135,28.,6.44419328073922));
#24421=CARTESIAN_POINT('Ctrl Pts',(143.175401713146,28.,6.60869565217392));
#24422=CARTESIAN_POINT('Ctrl Pts',(143.175401713146,28.622204314904,6.60869565217392));
#24423=CARTESIAN_POINT('Ctrl Pts',(143.054377037915,29.8642777153372,6.48707561474873));
#24424=CARTESIAN_POINT('Ctrl Pts',(142.448051488086,32.1203379370536,5.80658533410845));
#24425=CARTESIAN_POINT('Ctrl Pts',(141.409078045969,34.3900535537995,4.31115068270884));
#24426=CARTESIAN_POINT('Ctrl Pts',(140.46616862579,36.0628652143378,1.60758290672775));
#24427=CARTESIAN_POINT('Ctrl Pts',(140.461380759193,36.0690735156323,-1.24837379154744));
#24428=CARTESIAN_POINT('Ctrl Pts',(141.077842938275,34.9766629596617,-3.42496442652058));
#24429=CARTESIAN_POINT('Ctrl Pts',(141.828024497579,33.5000354399014,-4.9254108406999));
#24430=CARTESIAN_POINT('Ctrl Pts',(142.61406517216,31.5865966550244,-6.01113699999118));
#24431=CARTESIAN_POINT('Ctrl Pts',(143.198827571655,29.2764783425835,-6.63422718178349));
#24432=CARTESIAN_POINT('Ctrl Pts',(143.197512601211,26.7250000406644,-6.63359194555753));
#24433=CARTESIAN_POINT('Ctrl Pts',(142.51650955026,24.0303305797403,-5.90697582915808));
#24434=CARTESIAN_POINT('Ctrl Pts',(141.613773440736,22.0590093116005,-4.60669302069982));
#24435=CARTESIAN_POINT('Ctrl Pts',(140.940135198509,20.7760302225561,-2.96372789758379));
#24436=CARTESIAN_POINT('Ctrl Pts',(140.460722523566,19.9302298301654,-1.06990686592545));
#24437=CARTESIAN_POINT('Ctrl Pts',(140.466008212273,19.9365320616062,1.60770072303204));
#24438=CARTESIAN_POINT('Ctrl Pts',(141.407577159842,21.6081542657929,4.31108301914421));
#24439=CARTESIAN_POINT('Ctrl Pts',(142.44802175351,23.8795076799284,5.80658697436831));
#24440=CARTESIAN_POINT('Ctrl Pts',(143.05419832612,26.1354767285296,6.48707115577184));
#24441=CARTESIAN_POINT('Ctrl Pts',(143.175401713146,27.3777956850962,6.60869565217391));
#24442=CARTESIAN_POINT('Ctrl Pts',(143.175401713146,28.,6.60869565217391));
#24443=CARTESIAN_POINT('',(141.738644179071,28.,6.));
#24444=CARTESIAN_POINT('Origin',(141.738644179071,28.,8.));
#24445=CARTESIAN_POINT('Ctrl Pts',(141.738644179071,28.,6.));
#24446=CARTESIAN_POINT('Ctrl Pts',(141.738644179071,28.466653236178,6.));
#24447=CARTESIAN_POINT('Ctrl Pts',(141.592140624844,29.3982082865029,5.88958180812713));
#24448=CARTESIAN_POINT('Ctrl Pts',(140.858167590841,31.0902534527902,5.27176826386162));
#24449=CARTESIAN_POINT('Ctrl Pts',(139.600462897751,32.7925401653496,3.9140710145646));
#24450=CARTESIAN_POINT('Ctrl Pts',(138.45904623122,34.0471489107534,1.45951606005547));
#24451=CARTESIAN_POINT('Ctrl Pts',(138.453250392708,34.0518051367242,-1.13339199495755));
#24452=CARTESIAN_POINT('Ctrl Pts',(139.199494083175,33.2324972197463,-3.10950717670948));
#24453=CARTESIAN_POINT('Ctrl Pts',(140.107608602332,32.125026579926,-4.4717545790565));
#24454=CARTESIAN_POINT('Ctrl Pts',(141.059131524193,30.6899474912683,-5.45747964472883));
#24455=CARTESIAN_POINT('Ctrl Pts',(141.767001797266,28.9573587569376,-6.02317994135606));
#24456=CARTESIAN_POINT('Ctrl Pts',(141.76540999094,27.0437500304983,-6.02260321372987));
#24457=CARTESIAN_POINT('Ctrl Pts',(140.941037876631,25.0227479348052,-5.36291226594614));
#24458=CARTESIAN_POINT('Ctrl Pts',(139.848252059838,23.5442569837004,-4.18239234774062));
#24459=CARTESIAN_POINT('Ctrl Pts',(139.032795240301,22.5820226669171,-2.69075295964843));
#24460=CARTESIAN_POINT('Ctrl Pts',(138.452453581158,21.9476723726241,-0.97136281248494));
#24461=CARTESIAN_POINT('Ctrl Pts',(138.458852046436,21.9523990462047,1.45962302485803));
#24462=CARTESIAN_POINT('Ctrl Pts',(139.598646035598,23.2061156993447,3.91400958317042));
#24463=CARTESIAN_POINT('Ctrl Pts',(140.858131596355,24.9096307599463,5.27176975304492));
#24464=CARTESIAN_POINT('Ctrl Pts',(141.591924289514,26.6016075463972,5.88957775984548));
#24465=CARTESIAN_POINT('Ctrl Pts',(141.738644179071,27.533346763822,6.));
#24466=CARTESIAN_POINT('Ctrl Pts',(141.738644179071,28.,6.));
#24467=CARTESIAN_POINT('Origin',(129.8,28.,0.));
#24468=CARTESIAN_POINT('',(129.8,28.,6.));
#24469=CARTESIAN_POINT('Origin',(129.8,28.,0.));
#24470=CARTESIAN_POINT('',(129.8,28.,6.));
#24471=CARTESIAN_POINT('Origin',(127.8,26.5,-31.));
#24472=CARTESIAN_POINT('',(125.8,64.,-31.));
#24473=CARTESIAN_POINT('',(127.8,64.,-33.));
#24474=CARTESIAN_POINT('Origin',(127.8,64.,-31.));
#24475=CARTESIAN_POINT('',(127.8,59.9821371592664,-33.));
#24476=CARTESIAN_POINT('',(127.8,26.5,-33.));
#24477=CARTESIAN_POINT('',(125.8,57.9807621135332,-31.));
#24478=CARTESIAN_POINT('Ctrl Pts',(125.8,57.9807621135332,-31.));
#24479=CARTESIAN_POINT('Ctrl Pts',(125.8,57.982778257817,-31.0019400357417));
#24480=CARTESIAN_POINT('Ctrl Pts',(125.800002822804,57.9847942901491,-31.0038801895753));
#24481=CARTESIAN_POINT('Ctrl Pts',(125.80098220099,58.3344433583997,-31.3404084852548));
#24482=CARTESIAN_POINT('Ctrl Pts',(125.885795069427,58.6701680223804,-31.6705622861173));
#24483=CARTESIAN_POINT('Ctrl Pts',(126.152636007272,59.1545342172526,-32.1543180026666));
#24484=CARTESIAN_POINT('Ctrl Pts',(126.29212533093,59.3337989076212,-32.3354122100755));
#24485=CARTESIAN_POINT('Ctrl Pts',(126.64930385163,59.6459583395507,-32.6532332234622));
#24486=CARTESIAN_POINT('Ctrl Pts',(126.853946614142,59.7672434939641,-32.7780158331185));
#24487=CARTESIAN_POINT('Ctrl Pts',(127.208967246466,59.9010691778161,-32.9160577581802));
#24488=CARTESIAN_POINT('Ctrl Pts',(127.351252183116,59.9385021348617,-32.9548041970754));
#24489=CARTESIAN_POINT('Ctrl Pts',(127.59877150075,59.9747656314413,-32.9923574576679));
#24490=CARTESIAN_POINT('Ctrl Pts',(127.699058685214,59.9821371592665,-33.));
#24491=CARTESIAN_POINT('Ctrl Pts',(127.8,59.9821371592665,-33.));
#24492=CARTESIAN_POINT('',(125.8,26.5,-31.));
#24493=CARTESIAN_POINT('Origin',(127.8,64.,31.));
#24494=CARTESIAN_POINT('',(127.8,64.,33.));
#24495=CARTESIAN_POINT('Origin',(127.8,64.,31.));
#24496=CARTESIAN_POINT('',(125.8,64.,31.));
#24497=CARTESIAN_POINT('Origin',(127.8,64.,31.));
#24498=CARTESIAN_POINT('Origin',(127.8,64.,31.));
#24499=CARTESIAN_POINT('Origin',(127.8,64.,-16.5));
#24500=CARTESIAN_POINT('Origin',(127.8,64.,-31.));
#24501=CARTESIAN_POINT('',(125.8,64.,-16.5));
#24502=CARTESIAN_POINT('Origin',(127.8,26.5,31.));
#24503=CARTESIAN_POINT('',(125.8,57.9807621135332,31.));
#24504=CARTESIAN_POINT('',(127.8,59.9821371592664,33.));
#24505=CARTESIAN_POINT('Ctrl Pts',(127.8,59.9821371592664,33.));
#24506=CARTESIAN_POINT('Ctrl Pts',(127.699058685214,59.9821371592664,33.));
#24507=CARTESIAN_POINT('Ctrl Pts',(127.59877150075,59.9747656314413,32.9923574576679));
#24508=CARTESIAN_POINT('Ctrl Pts',(127.351252183116,59.9385021348617,32.9548041970754));
#24509=CARTESIAN_POINT('Ctrl Pts',(127.208967246466,59.9010691778161,32.9160577581802));
#24510=CARTESIAN_POINT('Ctrl Pts',(126.853946614143,59.7672434939644,32.7780158331189));
#24511=CARTESIAN_POINT('Ctrl Pts',(126.649303851631,59.6459583395513,32.6532332234628));
#24512=CARTESIAN_POINT('Ctrl Pts',(126.29212533093,59.3337989076212,32.3354122100755));
#24513=CARTESIAN_POINT('Ctrl Pts',(126.152636007272,59.1545342172527,32.1543180026667));
#24514=CARTESIAN_POINT('Ctrl Pts',(125.885795045952,58.6701679797686,31.6705622435593));
#24515=CARTESIAN_POINT('Ctrl Pts',(125.800982200837,58.3344433038848,31.3404084324536));
#24516=CARTESIAN_POINT('Ctrl Pts',(125.800002822804,57.9847942902325,31.0038801896633));
#24517=CARTESIAN_POINT('Ctrl Pts',(125.8,57.9827782577327,31.0019400356606));
#24518=CARTESIAN_POINT('Ctrl Pts',(125.8,57.9807621135332,31.));
#24519=CARTESIAN_POINT('',(127.8,26.5,33.));
#24520=CARTESIAN_POINT('',(125.8,26.5,31.));
#24521=CARTESIAN_POINT('Origin',(162.7,64.,31.));
#24522=CARTESIAN_POINT('',(173.,64.,33.));
#24523=CARTESIAN_POINT('Origin',(173.,64.,31.));
#24524=CARTESIAN_POINT('',(162.7,64.,33.));
#24525=CARTESIAN_POINT('Origin',(127.8,64.,-31.));
#24526=CARTESIAN_POINT('Origin',(127.8,64.,-31.));
#24527=CARTESIAN_POINT('Origin',(173.,26.5,31.));
#24528=CARTESIAN_POINT('Origin',(173.,64.,31.));
#24529=CARTESIAN_POINT('',(173.,59.9821371592664,33.));
#24530=CARTESIAN_POINT('',(173.,26.5,33.));
#24531=CARTESIAN_POINT('Ctrl Pts',(175.,57.9807621135332,31.));
#24532=CARTESIAN_POINT('Ctrl Pts',(175.,57.9827782576468,31.0019400355779));
#24533=CARTESIAN_POINT('Ctrl Pts',(174.999997177196,57.984794290312,31.0038801897477));
#24534=CARTESIAN_POINT('Ctrl Pts',(174.999017799316,58.3344432492304,31.3404083795179));
#24535=CARTESIAN_POINT('Ctrl Pts',(174.914204977582,58.6701679370494,31.6705622008938));
#24536=CARTESIAN_POINT('Ctrl Pts',(174.647363992729,59.1545342172525,32.1543180026665));
#24537=CARTESIAN_POINT('Ctrl Pts',(174.50787466907,59.3337989076211,32.3354122100754));
#24538=CARTESIAN_POINT('Ctrl Pts',(174.150696148369,59.6459583395515,32.6532332234631));
#24539=CARTESIAN_POINT('Ctrl Pts',(173.946053385857,59.7672434939645,32.778015833119));
#24540=CARTESIAN_POINT('Ctrl Pts',(173.591032753534,59.9010691778161,32.9160577581802));
#24541=CARTESIAN_POINT('Ctrl Pts',(173.448747816884,59.9385021348617,32.9548041970754));
#24542=CARTESIAN_POINT('Ctrl Pts',(173.20122849925,59.9747656314413,32.9923574576679));
#24543=CARTESIAN_POINT('Ctrl Pts',(173.100941314786,59.9821371592665,33.));
#24544=CARTESIAN_POINT('Ctrl Pts',(173.,59.9821371592665,33.));
#24545=CARTESIAN_POINT('Origin',(173.,64.,31.));
#24546=CARTESIAN_POINT('Origin',(173.,64.,31.));
#24547=CARTESIAN_POINT('Origin',(150.4,53.,-33.));
#24548=CARTESIAN_POINT('',(173.,64.,-33.));
#24549=CARTESIAN_POINT('',(162.7,64.,-33.));
#24550=CARTESIAN_POINT('',(173.,59.9821371592664,-33.));
#24551=CARTESIAN_POINT('',(173.,26.5,-33.));
#24552=CARTESIAN_POINT('',(125.8,59.9821371592664,-33.));
#24553=CARTESIAN_POINT('Origin',(162.7,64.,-31.));
#24554=CARTESIAN_POINT('Origin',(173.,64.,-31.));
#24555=CARTESIAN_POINT('Origin',(173.,64.,-16.5));
#24556=CARTESIAN_POINT('Origin',(173.,64.,-31.));
#24557=CARTESIAN_POINT('Origin',(127.8,-78.,40.));
#24558=CARTESIAN_POINT('Origin',(127.8,-78.,40.));
#24559=CARTESIAN_POINT('Origin',(127.8,-78.,-40.));
#24560=CARTESIAN_POINT('',(127.8,-78.,-42.));
#24561=CARTESIAN_POINT('Origin',(127.8,-78.,-40.));
#24562=CARTESIAN_POINT('Origin',(127.8,-78.,-40.));
#24563=CARTESIAN_POINT('Origin',(127.8,-30.,-40.));
#24564=CARTESIAN_POINT('',(125.8,-56.738633753706,-40.));
#24565=CARTESIAN_POINT('',(127.8,-58.153393661244,-42.));
#24566=CARTESIAN_POINT('Ctrl Pts',(127.8,-58.153393661244,-42.));
#24567=CARTESIAN_POINT('Ctrl Pts',(127.584791560318,-58.153393661244,-42.));
#24568=CARTESIAN_POINT('Ctrl Pts',(127.373410614215,-58.1295267522009,-41.9652805015393));
#24569=CARTESIAN_POINT('Ctrl Pts',(126.961480055368,-58.035764278849,-41.8294081195903));
#24570=CARTESIAN_POINT('Ctrl Pts',(126.768602924821,-57.9646256037392,-41.7265003535616));
#24571=CARTESIAN_POINT('Ctrl Pts',(126.401821931931,-57.7731997224245,-41.4513099318296));
#24572=CARTESIAN_POINT('Ctrl Pts',(126.239997043298,-57.6483119815763,-41.2726961269252));
#24573=CARTESIAN_POINT('Ctrl Pts',(126.009053039754,-57.3937106848192,-40.9118549730253));
#24574=CARTESIAN_POINT('Ctrl Pts',(125.930061060879,-57.2675944513766,-40.7342874762574));
#24575=CARTESIAN_POINT('Ctrl Pts',(125.826244922202,-57.0088681883845,-40.3729721347848));
#24576=CARTESIAN_POINT('Ctrl Pts',(125.800535718264,-56.8761189478115,-40.1889868307275));
#24577=CARTESIAN_POINT('Ctrl Pts',(125.800002761797,-56.7414261694738,-40.0038379708363));
#24578=CARTESIAN_POINT('Ctrl Pts',(125.8,-56.7400300001545,-40.0019189571955));
#24579=CARTESIAN_POINT('Ctrl Pts',(125.8,-56.738633753706,-40.));
#24580=CARTESIAN_POINT('',(127.8,-30.,-42.));
#24581=CARTESIAN_POINT('',(125.8,-30.,-40.));
#24582=CARTESIAN_POINT('Origin',(138.1,-78.,-40.));
#24583=CARTESIAN_POINT('',(173.,-78.,-42.));
#24584=CARTESIAN_POINT('',(138.1,-78.,-42.));
#24585=CARTESIAN_POINT('Origin',(173.,-78.,-40.));
#24586=CARTESIAN_POINT('',(138.1,-80.,-40.));
#24587=CARTESIAN_POINT('Origin',(173.,-78.,-40.));
#24588=CARTESIAN_POINT('Origin',(173.,-78.,-40.));
#24589=CARTESIAN_POINT('Origin',(173.,-78.,40.));
#24590=CARTESIAN_POINT('Origin',(173.,-78.,40.));
#24591=CARTESIAN_POINT('Origin',(127.8,-30.,40.));
#24592=CARTESIAN_POINT('',(127.8,-58.153393661244,42.));
#24593=CARTESIAN_POINT('',(125.8,-56.738633753706,40.));
#24594=CARTESIAN_POINT('Ctrl Pts',(125.8,-56.738633753706,40.));
#24595=CARTESIAN_POINT('Ctrl Pts',(125.8,-56.7400300001106,40.0019189571353));
#24596=CARTESIAN_POINT('Ctrl Pts',(125.800002761797,-56.7414261695115,40.0038379709001));
#24597=CARTESIAN_POINT('Ctrl Pts',(125.800535718258,-56.8761189462298,40.1889868282788));
#24598=CARTESIAN_POINT('Ctrl Pts',(125.826244922082,-57.008868188085,40.3729721343667));
#24599=CARTESIAN_POINT('Ctrl Pts',(125.930061060879,-57.2675944513765,40.7342874762574));
#24600=CARTESIAN_POINT('Ctrl Pts',(126.009053039754,-57.3937106848191,40.9118549730253));
#24601=CARTESIAN_POINT('Ctrl Pts',(126.239997043298,-57.6483119815763,41.2726961269252));
#24602=CARTESIAN_POINT('Ctrl Pts',(126.401821931931,-57.7731997224244,41.4513099318296));
#24603=CARTESIAN_POINT('Ctrl Pts',(126.768602924821,-57.9646256037392,41.7265003535616));
#24604=CARTESIAN_POINT('Ctrl Pts',(126.961480055368,-58.035764278849,41.8294081195903));
#24605=CARTESIAN_POINT('Ctrl Pts',(127.373410614215,-58.1295267522009,41.9652805015393));
#24606=CARTESIAN_POINT('Ctrl Pts',(127.584791560318,-58.153393661244,42.));
#24607=CARTESIAN_POINT('Ctrl Pts',(127.8,-58.153393661244,42.));
#24608=CARTESIAN_POINT('',(125.8,-30.,40.));
#24609=CARTESIAN_POINT('',(127.8,-30.,42.));
#24610=CARTESIAN_POINT('Origin',(173.,-30.,-40.));
#24611=CARTESIAN_POINT('',(173.,-30.,-42.));
#24612=CARTESIAN_POINT('Origin',(150.4,-60.,-42.));
#24613=CARTESIAN_POINT('',(125.8,-58.153393661244,-42.));
#24614=CARTESIAN_POINT('Origin',(125.8,-80.,-42.));
#24615=CARTESIAN_POINT('Origin',(125.8,0.,0.));
#24616=CARTESIAN_POINT('',(125.8,32.,-58.));
#24617=CARTESIAN_POINT('Origin',(125.8,32.,-32.));
#24618=CARTESIAN_POINT('',(125.8,-32.,-58.));
#24619=CARTESIAN_POINT('',(125.8,-16.,-58.));
#24620=CARTESIAN_POINT('Origin',(125.8,-32.,-32.));
#24621=CARTESIAN_POINT('',(125.8,-32.,58.));
#24622=CARTESIAN_POINT('Origin',(125.8,-32.,32.));
#24623=CARTESIAN_POINT('',(125.8,32.,58.));
#24624=CARTESIAN_POINT('',(125.8,16.,58.));
#24625=CARTESIAN_POINT('Origin',(125.8,32.,32.));
#24626=CARTESIAN_POINT('',(125.8,-5.51703383015883E-15,45.05));
#24627=CARTESIAN_POINT('Origin',(125.8,0.,0.));
#24628=CARTESIAN_POINT('',(125.8,-45.,-38.5));
#24629=CARTESIAN_POINT('Origin',(125.8,-45.,-45.));
#24630=CARTESIAN_POINT('',(125.8,45.,51.5));
#24631=CARTESIAN_POINT('Origin',(125.8,45.,45.));
#24632=CARTESIAN_POINT('',(125.8,-45.,51.5));
#24633=CARTESIAN_POINT('Origin',(125.8,-45.,45.));
#24634=CARTESIAN_POINT('',(125.8,45.,-38.5));
#24635=CARTESIAN_POINT('Origin',(125.8,45.,-45.));
#24636=CARTESIAN_POINT('Origin',(127.8,0.,0.));
#24637=CARTESIAN_POINT('',(127.8,-5.27210447032936E-15,43.05));
#24638=CARTESIAN_POINT('Origin',(127.8,-5.51703383015883E-15,45.05));
#24639=CARTESIAN_POINT('',(127.8,-43.05,-5.27210447032936E-15));
#24640=CARTESIAN_POINT('Origin',(127.8,0.,0.));
#24641=CARTESIAN_POINT('Origin',(127.8,0.,0.));
#24642=CARTESIAN_POINT('Origin',(127.75,0.,0.));
#24643=CARTESIAN_POINT('',(129.8,-43.05,-5.27210447032936E-15));
#24644=CARTESIAN_POINT('',(127.75,-43.05,-5.27210447032936E-15));
#24645=CARTESIAN_POINT('Origin',(129.8,0.,0.));
#24646=CARTESIAN_POINT('Origin',(127.8,-32.,-32.));
#24647=CARTESIAN_POINT('',(127.8,-32.,-60.));
#24648=CARTESIAN_POINT('Origin',(127.8,-32.,-58.));
#24649=CARTESIAN_POINT('Origin',(127.8,-32.,-32.));
#24650=CARTESIAN_POINT('Origin',(127.8,-16.,-58.));
#24651=CARTESIAN_POINT('',(127.8,32.,-60.));
#24652=CARTESIAN_POINT('Origin',(127.8,32.,-58.));
#24653=CARTESIAN_POINT('',(127.8,-16.,-60.));
#24654=CARTESIAN_POINT('Origin',(127.8,32.,-32.));
#24655=CARTESIAN_POINT('Origin',(127.8,32.,-32.));
#24656=CARTESIAN_POINT('Ctrl Pts',(131.,-20.,3.7470027081099E-15));
#24657=CARTESIAN_POINT('Ctrl Pts',(131.,-20.,0.861580403347816));
#24658=CARTESIAN_POINT('Ctrl Pts',(131.125764439308,-20.3550945008679,2.58493895098728));
#24659=CARTESIAN_POINT('Ctrl Pts',(131.558266830217,-21.7317216595771,4.69819302523181));
#24660=CARTESIAN_POINT('Ctrl Pts',(132.042509047825,-23.6963135961602,6.25318651247373));
#24661=CARTESIAN_POINT('Ctrl Pts',(132.368536443054,-25.8957266799623,7.08391599385498));
#24662=CARTESIAN_POINT('Ctrl Pts',(132.458664359226,-28.0044871996747,7.29993025650352));
#24663=CARTESIAN_POINT('Ctrl Pts',(132.380954794124,-29.8028754268023,7.11460122145983));
#24664=CARTESIAN_POINT('Ctrl Pts',(132.099300832929,-32.0502219061449,6.39759784836191));
#24665=CARTESIAN_POINT('Ctrl Pts',(131.659463837386,-33.8924146208701,5.09135905413439));
#24666=CARTESIAN_POINT('Ctrl Pts',(131.220675109436,-35.3580600016946,3.08054699453707));
#24667=CARTESIAN_POINT('Ctrl Pts',(130.959270175006,-36.1165905974382,0.896561407374775));
#24668=CARTESIAN_POINT('Ctrl Pts',(131.024509745219,-35.9339672140204,-1.76828950301325));
#24669=CARTESIAN_POINT('Ctrl Pts',(131.400892644271,-34.7994666629145,-4.05880603285176));
#24670=CARTESIAN_POINT('Ctrl Pts',(131.884794428522,-33.0159602268334,-5.7979751587154));
#24671=CARTESIAN_POINT('Ctrl Pts',(132.311702697533,-30.7087191160324,-6.95369978335721));
#24672=CARTESIAN_POINT('Ctrl Pts',(132.432701479047,-28.899900328133,-7.23809523809524));
#24673=CARTESIAN_POINT('Ctrl Pts',(132.432701479047,-28.,-7.23809523809524));
#24674=CARTESIAN_POINT('Ctrl Pts',(130.797619582017,-19.9116739443255,3.77151811328093E-15));
#24675=CARTESIAN_POINT('Ctrl Pts',(130.797619582017,-19.9116739443255,0.871444118239409));
#24676=CARTESIAN_POINT('Ctrl Pts',(130.904854620317,-20.2779548422433,2.61565600775496));
#24677=CARTESIAN_POINT('Ctrl Pts',(131.281531328409,-21.708188149755,4.72991862921347));
#24678=CARTESIAN_POINT('Ctrl Pts',(131.719414102451,-23.7218974853282,6.22503570820278));
#24679=CARTESIAN_POINT('Ctrl Pts',(132.028453321927,-25.9193631660258,6.98506280192702));
#24680=CARTESIAN_POINT('Ctrl Pts',(132.11587023659,-28.0042135305114,7.17959883876305));
#24681=CARTESIAN_POINT('Ctrl Pts',(132.040586744391,-29.7828553823862,7.0126779561723));
#24682=CARTESIAN_POINT('Ctrl Pts',(131.772280317266,-32.0212924370845,6.35840215413888));
#24683=CARTESIAN_POINT('Ctrl Pts',(131.371726605384,-33.9040625167872,5.11517750428116));
#24684=CARTESIAN_POINT('Ctrl Pts',(130.986964315205,-35.4241200681426,3.11366602926504));
#24685=CARTESIAN_POINT('Ctrl Pts',(130.762802930714,-36.2087539292741,0.907657337282378));
#24686=CARTESIAN_POINT('Ctrl Pts',(130.818337477733,-36.0207770197034,-1.78973624622093));
#24687=CARTESIAN_POINT('Ctrl Pts',(131.143137577146,-34.8435410607424,-4.09621049334934));
#24688=CARTESIAN_POINT('Ctrl Pts',(131.574530320972,-33.0022728031349,-5.79592783717056));
#24689=CARTESIAN_POINT('Ctrl Pts',(131.972813117268,-30.6784004498514,-6.86958311925421));
#24690=CARTESIAN_POINT('Ctrl Pts',(132.090706623172,-28.8898366829338,-7.12404769267738));
#24691=CARTESIAN_POINT('Ctrl Pts',(132.090706623172,-28.,-7.12404769267738));
#24692=CARTESIAN_POINT('Ctrl Pts',(130.422671463836,-19.6673355191975,3.85644558968536E-15));
#24693=CARTESIAN_POINT('Ctrl Pts',(130.422671463836,-19.6673355191975,0.89875912168986));
#24694=CARTESIAN_POINT('Ctrl Pts',(130.492531236214,-20.0479409376805,2.70000482740569));
#24695=CARTESIAN_POINT('Ctrl Pts',(130.746197220807,-21.5683467492021,4.86642730881123));
#24696=CARTESIAN_POINT('Ctrl Pts',(131.058780753502,-23.693411959482,6.31024557861326));
#24697=CARTESIAN_POINT('Ctrl Pts',(131.295887389147,-25.9273584681298,6.97089801517722));
#24698=CARTESIAN_POINT('Ctrl Pts',(131.365236878282,-28.003852058009,7.1324715976875));
#24699=CARTESIAN_POINT('Ctrl Pts',(131.30562358689,-29.7764177597774,6.99370296495644));
#24700=CARTESIAN_POINT('Ctrl Pts',(131.098323896218,-32.0392879611942,6.42935129116271));
#24701=CARTESIAN_POINT('Ctrl Pts',(130.809093968724,-34.0199081007393,5.24984625467384));
#24702=CARTESIAN_POINT('Ctrl Pts',(130.547361569822,-35.6366669116509,3.21270790048802));
#24703=CARTESIAN_POINT('Ctrl Pts',(130.400136757993,-36.4582322819073,0.935616039961515));
#24704=CARTESIAN_POINT('Ctrl Pts',(130.436222328538,-36.2637318150002,-1.84562949065027));
#24705=CARTESIAN_POINT('Ctrl Pts',(130.651675521466,-35.0205192781293,-4.22407147338777));
#24706=CARTESIAN_POINT('Ctrl Pts',(130.95294600974,-33.063483218923,-5.910694148768));
#24707=CARTESIAN_POINT('Ctrl Pts',(131.251356220669,-30.6692066978724,-6.87860346375511));
#24708=CARTESIAN_POINT('Ctrl Pts',(131.345673075562,-28.886528158348,-7.0862020745294));
#24709=CARTESIAN_POINT('Ctrl Pts',(131.345673075562,-28.,-7.0862020745294));
#24710=CARTESIAN_POINT('Ctrl Pts',(129.940396279447,-19.0495948139048,4.114252178675E-15));
#24711=CARTESIAN_POINT('Ctrl Pts',(129.940396279447,-19.0495948139048,0.967803292323193));
#24712=CARTESIAN_POINT('Ctrl Pts',(129.957030040264,-19.4304059125673,2.91217238551086));
#24713=CARTESIAN_POINT('Ctrl Pts',(130.02019438173,-21.0455248943075,5.3214716636252));
#24714=CARTESIAN_POINT('Ctrl Pts',(130.103911387302,-23.3810988218184,6.91455756751675));
#24715=CARTESIAN_POINT('Ctrl Pts',(130.172870889547,-25.8015110985969,7.58914966738149));
#24716=CARTESIAN_POINT('Ctrl Pts',(130.193826022536,-28.0039640203118,7.74532468216998));
#24717=CARTESIAN_POINT('Ctrl Pts',(130.175839613167,-29.8846980785751,7.61087423627512));
#24718=CARTESIAN_POINT('Ctrl Pts',(130.115043627593,-32.3241311937622,7.04038481196473));
#24719=CARTESIAN_POINT('Ctrl Pts',(130.036593186443,-34.5048871302672,5.74708243637949));
#24720=CARTESIAN_POINT('Ctrl Pts',(129.970485002834,-36.2397280762142,3.48005578751867));
#24721=CARTESIAN_POINT('Ctrl Pts',(129.934969533044,-37.0771971145615,1.00058657790848));
#24722=CARTESIAN_POINT('Ctrl Pts',(129.943526066177,-36.8840852946024,-1.97963074093526));
#24723=CARTESIAN_POINT('Ctrl Pts',(129.996191137842,-35.5908028312178,-4.60187443924087));
#24724=CARTESIAN_POINT('Ctrl Pts',(130.07473110145,-33.4523790881034,-6.48205257840886));
#24725=CARTESIAN_POINT('Ctrl Pts',(130.159228709516,-30.8349941080606,-7.50348217456204));
#24726=CARTESIAN_POINT('Ctrl Pts',(130.187841976599,-28.9404498479197,-7.70051204451168));
#24727=CARTESIAN_POINT('Ctrl Pts',(130.187841976599,-28.,-7.70051204451168));
#24728=CARTESIAN_POINT('Ctrl Pts',(129.8,-18.4981924307969,4.37121668877661E-15));
#24729=CARTESIAN_POINT('Ctrl Pts',(129.8,-18.4981924307969,1.02942794347193));
#24730=CARTESIAN_POINT('Ctrl Pts',(129.800425634876,-18.8638774763945,3.10110217056979));
#24731=CARTESIAN_POINT('Ctrl Pts',(129.800585502493,-20.5040688923186,5.77582141896866));
#24732=CARTESIAN_POINT('Ctrl Pts',(129.799595280034,-22.9901994383103,7.6330399323527));
#24733=CARTESIAN_POINT('Ctrl Pts',(129.798917565262,-25.6181226009167,8.45634664825776));
#24734=CARTESIAN_POINT('Ctrl Pts',(129.798497161429,-28.0045440318595,8.64969573564895));
#24735=CARTESIAN_POINT('Ctrl Pts',(129.798915409572,-30.0419010743684,8.48314284965744));
#24736=CARTESIAN_POINT('Ctrl Pts',(129.79980293301,-32.6909142565747,7.78606205295877));
#24737=CARTESIAN_POINT('Ctrl Pts',(129.800236816359,-35.0235999478161,6.26044328157787));
#24738=CARTESIAN_POINT('Ctrl Pts',(129.801004712256,-36.8063771223098,3.72609760124849));
#24739=CARTESIAN_POINT('Ctrl Pts',(129.800987139019,-37.6246741986015,1.0561663884385));
#24740=CARTESIAN_POINT('Ctrl Pts',(129.801204967059,-37.440405596014,-2.09611264808735));
#24741=CARTESIAN_POINT('Ctrl Pts',(129.801021929527,-36.1533892376718,-4.96274944615673));
#24742=CARTESIAN_POINT('Ctrl Pts',(129.800421486173,-33.9066423575678,-7.11924690888942));
#24743=CARTESIAN_POINT('Ctrl Pts',(129.799758219885,-31.0743896288208,-8.34843617812973));
#24744=CARTESIAN_POINT('Ctrl Pts',(129.8,-29.0188558496653,-8.59461511716011));
#24745=CARTESIAN_POINT('Ctrl Pts',(129.8,-28.,-8.59461511716011));
#24746=CARTESIAN_POINT('Ctrl Pts',(129.8,-18.1669697220177,4.53337703798322E-15));
#24747=CARTESIAN_POINT('Ctrl Pts',(129.8,-18.1669697220177,1.06646420912009));
#24748=CARTESIAN_POINT('Ctrl Pts',(129.8,-18.5235013453798,3.2144015031083));
#24749=CARTESIAN_POINT('Ctrl Pts',(129.8,-20.1781424757955,6.04867179819866));
#24750=CARTESIAN_POINT('Ctrl Pts',(129.8,-22.7540398357438,8.06622528687979));
#24751=CARTESIAN_POINT('Ctrl Pts',(129.8,-25.5068213458088,8.98108454885427));
#24752=CARTESIAN_POINT('Ctrl Pts',(129.8,-28.0048708711283,9.19767148720769));
#24753=CARTESIAN_POINT('Ctrl Pts',(129.8,-30.1372432217561,9.01104409835271));
#24754=CARTESIAN_POINT('Ctrl Pts',(129.8,-32.912704492555,8.23578485682426));
#24755=CARTESIAN_POINT('Ctrl Pts',(129.8,-35.3359659106613,6.56920417867618));
#24756=CARTESIAN_POINT('Ctrl Pts',(129.8,-37.1469121757438,3.87368039798568));
#24757=CARTESIAN_POINT('Ctrl Pts',(129.8,-37.9534190391165,1.0894602487521));
#24758=CARTESIAN_POINT('Ctrl Pts',(129.8,-37.7745232552706,-2.16589095067385));
#24759=CARTESIAN_POINT('Ctrl Pts',(129.8,-36.4917024138616,-5.17924099653794));
#24760=CARTESIAN_POINT('Ctrl Pts',(129.8,-34.1806914538042,-7.5027269121639));
#24761=CARTESIAN_POINT('Ctrl Pts',(129.8,-31.2194942135712,-8.85890855860159));
#24762=CARTESIAN_POINT('Ctrl Pts',(129.8,-29.0664642091201,-9.13537983414592));
#24763=CARTESIAN_POINT('Ctrl Pts',(129.8,-28.,-9.13537983414592));
#24764=CARTESIAN_POINT('',(129.8,-28.,-9.13537983414592));
#24765=CARTESIAN_POINT('Origin',(131.8,-28.,-9.13537983414592));
#24766=CARTESIAN_POINT('',(129.8,-18.1669697220177,4.71844785465692E-15));
#24767=CARTESIAN_POINT('Ctrl Pts',(129.8,-28.,-9.13537983414592));
#24768=CARTESIAN_POINT('Ctrl Pts',(129.8,-28.2710934566237,-9.13537983414592));
#24769=CARTESIAN_POINT('Ctrl Pts',(129.800000000254,-28.5423900297121,-9.12631611496261));
#24770=CARTESIAN_POINT('Ctrl Pts',(129.800000010001,-28.8129549506681,-9.1080974690796));
#24771=CARTESIAN_POINT('Ctrl Pts',(129.800000012749,-28.8892548171417,-9.1029597733159));
#24772=CARTESIAN_POINT('Ctrl Pts',(129.800000016053,-28.9654968054901,-9.09709411794451));
#24773=CARTESIAN_POINT('Ctrl Pts',(129.800000019417,-29.0416606814196,-9.09049862323265));
#24774=CARTESIAN_POINT('Ctrl Pts',(129.800000030122,-29.284030104473,-9.0695103761331));
#24775=CARTESIAN_POINT('Ctrl Pts',(129.800000031778,-29.5265914722412,-9.04108367787807));
#24776=CARTESIAN_POINT('Ctrl Pts',(129.800000024833,-29.7684741621524,-9.00491149302646));
#24777=CARTESIAN_POINT('Ctrl Pts',(129.800000018035,-30.0052379902963,-8.96950480492925));
#24778=CARTESIAN_POINT('Ctrl Pts',(129.800000005335,-30.2413508050631,-8.92667677470373));
#24779=CARTESIAN_POINT('Ctrl Pts',(129.799999997683,-30.4759872992535,-8.87618791384607));
#24780=CARTESIAN_POINT('Ctrl Pts',(129.799999990032,-30.710623793444,-8.82569905298842));
#24781=CARTESIAN_POINT('Ctrl Pts',(129.799999987709,-30.9437832422619,-8.76754899956281));
#24782=CARTESIAN_POINT('Ctrl Pts',(129.799999993066,-31.1746424139292,-8.70155180091808));
#24783=CARTESIAN_POINT('Ctrl Pts',(129.799999998169,-31.3945493990912,-8.63868557438573));
#24784=CARTESIAN_POINT('Ctrl Pts',(129.800000008838,-31.6123685851659,-8.56869932574673));
#24785=CARTESIAN_POINT('Ctrl Pts',(129.800000024788,-31.827313863548,-8.49162045592886));
#24786=CARTESIAN_POINT('Ctrl Pts',(129.800000040296,-32.0362926162709,-8.41668116813863));
#24787=CARTESIAN_POINT('Ctrl Pts',(129.800000059864,-32.2425542680841,-8.33503768846553));
#24788=CARTESIAN_POINT('Ctrl Pts',(129.800000101707,-32.4453954742136,-8.24676010058969));
#24789=CARTESIAN_POINT('Ctrl Pts',(129.800000128327,-32.5744395368168,-8.19059942794497));
#24790=CARTESIAN_POINT('Ctrl Pts',(129.800000164393,-32.7020996550235,-8.13175463808071));
#24791=CARTESIAN_POINT('Ctrl Pts',(129.80000022104,-32.8282003906212,-8.07025328042285));
#24792=CARTESIAN_POINT('Ctrl Pts',(129.800000300864,-33.0058933182513,-7.98358958061452));
#24793=CARTESIAN_POINT('Ctrl Pts',(129.800000377488,-33.1814457993943,-7.89126827704086));
#24794=CARTESIAN_POINT('Ctrl Pts',(129.800000431821,-33.3542076956327,-7.79326454350896));
#24795=CARTESIAN_POINT('Ctrl Pts',(129.800000484865,-33.5228719225701,-7.69758532075768));
#24796=CARTESIAN_POINT('Ctrl Pts',(129.800000517254,-33.6888758343857,-7.59649010717235));
#24797=CARTESIAN_POINT('Ctrl Pts',(129.800000528243,-33.8516287624338,-7.49000317241242));
#24798=CARTESIAN_POINT('Ctrl Pts',(129.800000533251,-33.9257891309385,-7.44148109408528));
#24799=CARTESIAN_POINT('Ctrl Pts',(129.800000533999,-33.9992747513072,-7.39184019488646));
#24800=CARTESIAN_POINT('Ctrl Pts',(129.80000053125,-34.072031219817,-7.34108608127361));
#24801=CARTESIAN_POINT('Ctrl Pts',(129.800000525348,-34.2282038085113,-7.23214179807585));
#24802=CARTESIAN_POINT('Ctrl Pts',(129.800000502802,-34.3810149199932,-7.11806550802202));
#24803=CARTESIAN_POINT('Ctrl Pts',(129.800000478449,-34.5299490544096,-6.9992289330591));
#24804=CARTESIAN_POINT('Ctrl Pts',(129.800000454184,-34.6783469214609,-6.88082025313308));
#24805=CARTESIAN_POINT('Ctrl Pts',(129.800000428039,-34.8228951901582,-6.75768588000836));
#24806=CARTESIAN_POINT('Ctrl Pts',(129.800000423516,-34.9631160169095,-6.63023387127949));
#24807=CARTESIAN_POINT('Ctrl Pts',(129.800000419042,-35.1018396307111,-6.50414273598408));
#24808=CARTESIAN_POINT('Ctrl Pts',(129.800000435551,-35.2363273181619,-6.3738260917508));
#24809=CARTESIAN_POINT('Ctrl Pts',(129.8000005065,-35.3661544469235,-6.23971268446155));
#24810=CARTESIAN_POINT('Ctrl Pts',(129.800000542169,-35.4314254897008,-6.17228670017229));
#24811=CARTESIAN_POINT('Ctrl Pts',(129.800000591785,-35.4955191647688,-6.10390153542689));
#24812=CARTESIAN_POINT('Ctrl Pts',(129.800000660874,-35.5583856847107,-6.03461443125748));
#24813=CARTESIAN_POINT('Ctrl Pts',(129.800000797243,-35.6824729005216,-5.89785413569915));
#24814=CARTESIAN_POINT('Ctrl Pts',(129.800000888877,-35.8026304832297,-5.75672551648309));
#24815=CARTESIAN_POINT('Ctrl Pts',(129.800000933592,-35.9183208388435,-5.61155087902511));
#24816=CARTESIAN_POINT('Ctrl Pts',(129.800000978028,-36.0332901024865,-5.46728110753362));
#24817=CARTESIAN_POINT('Ctrl Pts',(129.800000976557,-36.1438471657959,-5.31901594976647));
#24818=CARTESIAN_POINT('Ctrl Pts',(129.800000939261,-36.2494959453691,-5.16711228046974));
#24819=CARTESIAN_POINT('Ctrl Pts',(129.800000930872,-36.2732595707179,-5.1329445229163));
#24820=CARTESIAN_POINT('Ctrl Pts',(129.800000920706,-36.2967750114404,-5.09859283065372));
#24821=CARTESIAN_POINT('Ctrl Pts',(129.800000908934,-36.3200368825082,-5.06406152131753));
#24822=CARTESIAN_POINT('Ctrl Pts',(129.800000856842,-36.4229671442463,-4.91126569944354));
#24823=CARTESIAN_POINT('Ctrl Pts',(129.800000772968,-36.5209292387116,-4.7549505850943));
#24824=CARTESIAN_POINT('Ctrl Pts',(129.800000675395,-36.6137381843152,-4.59565457927221));
#24825=CARTESIAN_POINT('Ctrl Pts',(129.800000576889,-36.7074355362313,-4.43483372499716));
#24826=CARTESIAN_POINT('Ctrl Pts',(129.800000464575,-36.79588042377,-4.27097517140965));
#24827=CARTESIAN_POINT('Ctrl Pts',(129.800000359853,-36.8789285269501,-4.1046607860374));
#24828=CARTESIAN_POINT('Ctrl Pts',(129.800000254053,-36.9628311829886,-3.93663504991831));
#24829=CARTESIAN_POINT('Ctrl Pts',(129.800000156076,-37.0412252425313,-3.76610326411397));
#24830=CARTESIAN_POINT('Ctrl Pts',(129.80000008911,-37.1140114128655,-3.59368526445729));
#24831=CARTESIAN_POINT('Ctrl Pts',(129.800000034074,-37.1738304260567,-3.45198424421535));
#24832=CARTESIAN_POINT('Ctrl Pts',(129.8,-37.2298625958302,-3.30900973845834));
#24833=CARTESIAN_POINT('Ctrl Pts',(129.8,-37.2820785495145,-3.16511141418121));
#24834=CARTESIAN_POINT('Ctrl Pts',(129.8,-37.3484560294473,-2.98218632217128));
#24835=CARTESIAN_POINT('Ctrl Pts',(129.800000080133,-37.4091007452409,-2.79654512834284));
#24836=CARTESIAN_POINT('Ctrl Pts',(129.800000206248,-37.4637959430478,-2.60880501888571));
#24837=CARTESIAN_POINT('Ctrl Pts',(129.800000313534,-37.5103245663064,-2.44909650381115));
#24838=CARTESIAN_POINT('Ctrl Pts',(129.800000454017,-37.5525484091508,-2.28786975503681));
#24839=CARTESIAN_POINT('Ctrl Pts',(129.800000603747,-37.5903609896446,-2.12551710040222));
#24840=CARTESIAN_POINT('Ctrl Pts',(129.800000781187,-37.6351715920225,-1.93311763554626));
#24841=CARTESIAN_POINT('Ctrl Pts',(129.800000971388,-37.6737856845845,-1.73913712095642));
#24842=CARTESIAN_POINT('Ctrl Pts',(129.800001132302,-37.7061703661713,-1.54415505986223));
#24843=CARTESIAN_POINT('Ctrl Pts',(129.800001293741,-37.738660806647,-1.34853624444055));
#24844=CARTESIAN_POINT('Ctrl Pts',(129.800001425367,-37.7648810751542,-1.15190984292285));
#24845=CARTESIAN_POINT('Ctrl Pts',(129.800001486965,-37.784850221988,-0.954867005853932));
#24846=CARTESIAN_POINT('Ctrl Pts',(129.800001548546,-37.804813802462,-0.757879094082963));
#24847=CARTESIAN_POINT('Ctrl Pts',(129.800001539778,-37.8185297813407,-0.560475514225451));
#24848=CARTESIAN_POINT('Ctrl Pts',(129.800001427913,-37.8260690978795,-0.363244978850374));
#24849=CARTESIAN_POINT('Ctrl Pts',(129.800001359466,-37.830682188985,-0.242565282781485));
#24850=CARTESIAN_POINT('Ctrl Pts',(129.800001252581,-37.832983833148,-0.121950301222289));
#24851=CARTESIAN_POINT('Ctrl Pts',(129.800001102091,-37.8329997684066,-0.0015332147094816));
#24852=CARTESIAN_POINT('Ctrl Pts',(129.800000850592,-37.8330263993663,0.199707484668333));
#24853=CARTESIAN_POINT('Ctrl Pts',(129.800000660673,-37.8266123822281,0.401429055739714));
#24854=CARTESIAN_POINT('Ctrl Pts',(129.800000514432,-37.8137142562269,0.603017950828346));
#24855=CARTESIAN_POINT('Ctrl Pts',(129.80000040164,-37.8037663599371,0.758496771653588));
#24856=CARTESIAN_POINT('Ctrl Pts',(129.800000314902,-37.7899624204569,0.913896383862366));
#24857=CARTESIAN_POINT('Ctrl Pts',(129.800000247285,-37.7723036328808,1.06893400987562));
#24858=CARTESIAN_POINT('Ctrl Pts',(129.800000159877,-37.7494761710609,1.26935068475925));
#24859=CARTESIAN_POINT('Ctrl Pts',(129.800000104285,-37.7202053021452,1.46916194084438));
#24860=CARTESIAN_POINT('Ctrl Pts',(129.800000068028,-37.6845214547503,1.66772072705263));
#24861=CARTESIAN_POINT('Ctrl Pts',(129.80000003226,-37.6493197354518,1.86359676527837));
#24862=CARTESIAN_POINT('Ctrl Pts',(129.800000015447,-37.6078772734481,2.05825340593417));
#24863=CARTESIAN_POINT('Ctrl Pts',(129.80000000739,-37.5602721024491,2.25108112394059));
#24864=CARTESIAN_POINT('Ctrl Pts',(129.799999999959,-37.5163647521297,2.42893058836005));
#24865=CARTESIAN_POINT('Ctrl Pts',(129.8,-37.467215437465,2.60522401819515));
#24866=CARTESIAN_POINT('Ctrl Pts',(129.8,-37.4129218132307,2.77949806312598));
#24867=CARTESIAN_POINT('Ctrl Pts',(129.8,-37.3553984417258,2.96413909182102));
#24868=CARTESIAN_POINT('Ctrl Pts',(129.800000073857,-37.2917719965685,3.14747629098194));
#24869=CARTESIAN_POINT('Ctrl Pts',(129.800000184787,-37.2220351869846,3.32888387880954));
#24870=CARTESIAN_POINT('Ctrl Pts',(129.800000294156,-37.153279774552,3.50773854098737));
#24871=CARTESIAN_POINT('Ctrl Pts',(129.800000439685,-37.0785848646926,3.68471697306431));
#24872=CARTESIAN_POINT('Ctrl Pts',(129.800000584987,-36.9979923490264,3.85923182135913));
#24873=CARTESIAN_POINT('Ctrl Pts',(129.800000661901,-36.9553317214072,3.9516090464101));
#24874=CARTESIAN_POINT('Ctrl Pts',(129.800000738712,-36.9110194144865,4.04329623882756));
#24875=CARTESIAN_POINT('Ctrl Pts',(129.800000809976,-36.8650671546441,4.13420850839983));
#24876=CARTESIAN_POINT('Ctrl Pts',(129.800000942579,-36.7795634823621,4.30336956664946));
#24877=CARTESIAN_POINT('Ctrl Pts',(129.800001055026,-36.6883793253902,4.46984592494155));
#24878=CARTESIAN_POINT('Ctrl Pts',(129.800001121067,-36.5918570142447,4.63306960800581));
#24879=CARTESIAN_POINT('Ctrl Pts',(129.800001186835,-36.4957337566541,4.79561847309071));
#24880=CARTESIAN_POINT('Ctrl Pts',(129.8000012062,-36.3943167793967,4.95494097982122));
#24881=CARTESIAN_POINT('Ctrl Pts',(129.800001168723,-36.2879846568996,5.11050799627058));
#24882=CARTESIAN_POINT('Ctrl Pts',(129.800001131667,-36.1828466404151,5.26432800057223));
#24883=CARTESIAN_POINT('Ctrl Pts',(129.800001038672,-36.0729036737357,5.41447597179017));
#24884=CARTESIAN_POINT('Ctrl Pts',(129.800000900192,-35.9585552994893,5.56047849998203));
#24885=CARTESIAN_POINT('Ctrl Pts',(129.800000840922,-35.909613657967,5.62296826814189));
#24886=CARTESIAN_POINT('Ctrl Pts',(129.80000077361,-35.8598653835609,5.68469915576676));
#24887=CARTESIAN_POINT('Ctrl Pts',(129.800000700539,-35.8093434235041,5.74563649233914));
#24888=CARTESIAN_POINT('Ctrl Pts',(129.800000634558,-35.7637237600527,5.80066089723016));
#24889=CARTESIAN_POINT('Ctrl Pts',(129.800000575695,-35.7173576466735,5.85516476191921));
#24890=CARTESIAN_POINT('Ctrl Pts',(129.800000523201,-35.6702606155969,5.90911300404228));
#24891=CARTESIAN_POINT('Ctrl Pts',(129.800000390178,-35.5509152099631,6.04581960087493));
#24892=CARTESIAN_POINT('Ctrl Pts',(129.800000297889,-35.4268732339045,6.17895614192948));
#24893=CARTESIAN_POINT('Ctrl Pts',(129.800000232082,-35.2985279351237,6.30821965909818));
#24894=CARTESIAN_POINT('Ctrl Pts',(129.80000016534,-35.1683606080414,6.43931823987149));
#24895=CARTESIAN_POINT('Ctrl Pts',(129.800000125829,-35.0337672516901,6.56643278619385));
#24896=CARTESIAN_POINT('Ctrl Pts',(129.800000100224,-34.8952005298572,6.68928022189627));
#24897=CARTESIAN_POINT('Ctrl Pts',(129.800000074127,-34.7539689311153,6.81449022553994));
#24898=CARTESIAN_POINT('Ctrl Pts',(129.800000062456,-34.608610051288,6.93526709679275));
#24899=CARTESIAN_POINT('Ctrl Pts',(129.800000052925,-34.4596414349555,7.05134961948229));
#24900=CARTESIAN_POINT('Ctrl Pts',(129.800000043317,-34.3094768861733,7.16836406232483));
#24901=CARTESIAN_POINT('Ctrl Pts',(129.800000035855,-34.1556449145912,7.2806082323216));
#24902=CARTESIAN_POINT('Ctrl Pts',(129.800000020148,-33.9987072694013,7.38785752401803));
#24903=CARTESIAN_POINT('Ctrl Pts',(129.800000004335,-33.840706859907,7.49583309600724));
#24904=CARTESIAN_POINT('Ctrl Pts',(129.799999980125,-33.6795591174923,7.59874567871118));
#24905=CARTESIAN_POINT('Ctrl Pts',(129.799999939642,-33.5158612568849,7.6964130662455));
#24906=CARTESIAN_POINT('Ctrl Pts',(129.799999916495,-33.4222649849815,7.75225560032523));
#24907=CARTESIAN_POINT('Ctrl Pts',(129.799999888082,-33.3278354427798,7.80638429637383));
#24908=CARTESIAN_POINT('Ctrl Pts',(129.799999853411,-33.23268668598,7.85877235429687));
#24909=CARTESIAN_POINT('Ctrl Pts',(129.799999781276,-33.0347260541761,7.96776771476434));
#24910=CARTESIAN_POINT('Ctrl Pts',(129.799999677419,-32.8323207055757,8.07008926509624));
#24911=CARTESIAN_POINT('Ctrl Pts',(129.799999565654,-32.6261658853824,8.16533300337038));
#24912=CARTESIAN_POINT('Ctrl Pts',(129.799999487616,-32.482222004947,8.23183522369922));
#24913=CARTESIAN_POINT('Ctrl Pts',(129.799999406892,-32.3364511385822,8.29488741902412));
#24914=CARTESIAN_POINT('Ctrl Pts',(129.799999337055,-32.1891014570786,8.35436170891443));
#24915=CARTESIAN_POINT('Ctrl Pts',(129.799999236438,-31.9768103954567,8.44004808442058));
#24916=CARTESIAN_POINT('Ctrl Pts',(129.799999161317,-31.7612410327654,8.51830550156099));
#24917=CARTESIAN_POINT('Ctrl Pts',(129.799999142915,-31.5432184156714,8.58928340104066));
#24918=CARTESIAN_POINT('Ctrl Pts',(129.799999123369,-31.311641829312,8.6646738347835));
#24919=CARTESIAN_POINT('Ctrl Pts',(129.799999170399,-31.0772979987876,8.73185120061919));
#24920=CARTESIAN_POINT('Ctrl Pts',(129.799999253853,-30.8412069558948,8.7910483680274));
#24921=CARTESIAN_POINT('Ctrl Pts',(129.799999337306,-30.605115913002,8.85024553543562));
#24922=CARTESIAN_POINT('Ctrl Pts',(129.79999945547,-30.3672786267893,8.90146272598421));
#24923=CARTESIAN_POINT('Ctrl Pts',(129.799999505143,-30.1287336314256,8.94498489058459));
#24924=CARTESIAN_POINT('Ctrl Pts',(129.799999540572,-29.9585896989811,8.97602738729393));
#24925=CARTESIAN_POINT('Ctrl Pts',(129.799999538851,-29.7880859291832,9.00315616367553));
#24926=CARTESIAN_POINT('Ctrl Pts',(129.799999455305,-29.6174044031091,9.02642322783757));
#24927=CARTESIAN_POINT('Ctrl Pts',(129.799999350579,-29.4034531173255,9.05558876442715));
#24928=CARTESIAN_POINT('Ctrl Pts',(129.799999255948,-29.1884321010775,9.07885974035984));
#24929=CARTESIAN_POINT('Ctrl Pts',(129.799999182402,-28.9727587444094,9.09626194566826));
#24930=CARTESIAN_POINT('Ctrl Pts',(129.799999107835,-28.754089276615,9.11390590054535));
#24931=CARTESIAN_POINT('Ctrl Pts',(129.799999055151,-28.5347494923584,9.12551691582513));
#24932=CARTESIAN_POINT('Ctrl Pts',(129.799999033247,-28.3151806182946,9.13117521678299));
#24933=CARTESIAN_POINT('Ctrl Pts',(129.799999022883,-28.2112899535657,9.13385248445244));
#24934=CARTESIAN_POINT('Ctrl Pts',(129.799999019353,-28.1073480637685,9.13519783447652));
#24935=CARTESIAN_POINT('Ctrl Pts',(129.799999023188,-28.00340188464,9.13522380628829));
#24936=CARTESIAN_POINT('Ctrl Pts',(129.799999031191,-27.7864545244573,9.13527801237889));
#24937=CARTESIAN_POINT('Ctrl Pts',(129.7999990716,-27.5694888171688,9.12958168360609));
#24938=CARTESIAN_POINT('Ctrl Pts',(129.799999140631,-27.3530624253067,9.11804672246127));
#24939=CARTESIAN_POINT('Ctrl Pts',(129.799999197848,-27.1736750413013,9.10848584364899));
#24940=CARTESIAN_POINT('Ctrl Pts',(129.799999274552,-26.9946582756265,9.0949146064092));
#24941=CARTESIAN_POINT('Ctrl Pts',(129.799999366665,-26.8163256593467,9.07730975400949));
#24942=CARTESIAN_POINT('Ctrl Pts',(129.799999489158,-26.5791782143552,9.05389874903946));
#24943=CARTESIAN_POINT('Ctrl Pts',(129.799999545856,-26.341981406837,9.02318864976405));
#24944=CARTESIAN_POINT('Ctrl Pts',(129.799999563548,-26.1054113455679,8.98495051838404));
#24945=CARTESIAN_POINT('Ctrl Pts',(129.799999569323,-26.0281782992592,8.97246691265732));
#24946=CARTESIAN_POINT('Ctrl Pts',(129.799999571014,-25.9510120755735,8.95918135914482));
#24947=CARTESIAN_POINT('Ctrl Pts',(129.799999569641,-25.8739362147895,8.94508710392248));
#24948=CARTESIAN_POINT('Ctrl Pts',(129.799999565518,-25.642349894167,8.90273873861512));
#24949=CARTESIAN_POINT('Ctrl Pts',(129.799999534226,-25.4115797248202,8.85308564139544));
#24950=CARTESIAN_POINT('Ctrl Pts',(129.799999501623,-25.1825202534547,8.79599159960173));
#24951=CARTESIAN_POINT('Ctrl Pts',(129.799999470053,-24.9607149557348,8.74070569126275));
#24952=CARTESIAN_POINT('Ctrl Pts',(129.799999437428,-24.7405143972207,8.67844279562064));
#24953=CARTESIAN_POINT('Ctrl Pts',(129.799999419512,-24.5227201485777,8.60912629937209));
#24954=CARTESIAN_POINT('Ctrl Pts',(129.799999401972,-24.3094819864445,8.54125985038344));
#24955=CARTESIAN_POINT('Ctrl Pts',(129.799999398573,-24.0985510812376,8.46663187188181));
#24956=CARTESIAN_POINT('Ctrl Pts',(129.799999415083,-23.8906602834359,8.3852152288404));
#24957=CARTESIAN_POINT('Ctrl Pts',(129.799999431062,-23.6894508000853,8.30641520086551));
#24958=CARTESIAN_POINT('Ctrl Pts',(129.79999946563,-23.4910895506826,8.22125598847036));
#24959=CARTESIAN_POINT('Ctrl Pts',(129.799999515702,-23.2962156528616,8.12975391530791));
#24960=CARTESIAN_POINT('Ctrl Pts',(129.799999555263,-23.1422443023712,8.05745743058098));
#24961=CARTESIAN_POINT('Ctrl Pts',(129.799999604328,-22.9904495947184,7.9812020624661));
#24962=CARTESIAN_POINT('Ctrl Pts',(129.799999657982,-22.8411326305199,7.90101415297964));
#24963=CARTESIAN_POINT('Ctrl Pts',(129.799999658949,-22.8384421833811,7.89956929818495));
#24964=CARTESIAN_POINT('Ctrl Pts',(129.799999659917,-22.835752540291,7.89812316708923));
#24965=CARTESIAN_POINT('Ctrl Pts',(129.799999660887,-22.8330637030347,7.89667576089017));
#24966=CARTESIAN_POINT('Ctrl Pts',(129.799999722439,-22.662362016112,7.80478671878978));
#24967=CARTESIAN_POINT('Ctrl Pts',(129.799999764999,-22.4939452362869,7.70717170981652));
#24968=CARTESIAN_POINT('Ctrl Pts',(129.799999830609,-22.3284431873294,7.60404124706532));
#24969=CARTESIAN_POINT('Ctrl Pts',(129.799999896216,-22.1629494633321,7.50091597190547));
#24970=CARTESIAN_POINT('Ctrl Pts',(129.799999986085,-22.0003707418458,7.39227607036555));
#24971=CARTESIAN_POINT('Ctrl Pts',(129.800000113347,-21.8413151221296,7.27837928976005));
#24972=CARTESIAN_POINT('Ctrl Pts',(129.80000023931,-21.6838841539901,7.16564589202987));
#24973=CARTESIAN_POINT('Ctrl Pts',(129.80000040171,-21.5299051675592,7.04776279374741));
#24974=CARTESIAN_POINT('Ctrl Pts',(129.800000577888,-21.3799388716861,6.92502157913105));
#24975=CARTESIAN_POINT('Ctrl Pts',(129.800000752308,-21.2314688855212,6.80350503216388));
#24976=CARTESIAN_POINT('Ctrl Pts',(129.80000093908,-21.0869323471168,6.67722713868374));
#24977=CARTESIAN_POINT('Ctrl Pts',(129.800001091748,-20.9468380388716,6.54650711065002));
#24978=CARTESIAN_POINT('Ctrl Pts',(129.800001241687,-20.809247390563,6.41812321247912));
#24979=CARTESIAN_POINT('Ctrl Pts',(129.800001357032,-20.6759419276993,6.28545484859302));
#24980=CARTESIAN_POINT('Ctrl Pts',(129.800001391451,-20.5473640076158,6.14883492474288));
#24981=CARTESIAN_POINT('Ctrl Pts',(129.800001411037,-20.4741943462765,6.07108881130586));
#24982=CARTESIAN_POINT('Ctrl Pts',(129.800001404497,-20.4025548953712,5.99206356141718));
#24983=CARTESIAN_POINT('Ctrl Pts',(129.800001366462,-20.3325207155241,5.9118244915949));
#24984=CARTESIAN_POINT('Ctrl Pts',(129.80000132551,-20.2571173524217,5.82543387875396));
#24985=CARTESIAN_POINT('Ctrl Pts',(129.80000124789,-20.1835748674122,5.73763626889217));
#24986=CARTESIAN_POINT('Ctrl Pts',(129.800001133642,-20.1119397099029,5.64856846558855));
#24987=CARTESIAN_POINT('Ctrl Pts',(129.800000941388,-19.9913933626716,5.49868677735778));
#24988=CARTESIAN_POINT('Ctrl Pts',(129.800000802801,-19.8755809187763,5.34420807272763));
#24989=CARTESIAN_POINT('Ctrl Pts',(129.800000704905,-19.7648729658217,5.18565120424431));
#24990=CARTESIAN_POINT('Ctrl Pts',(129.800000605327,-19.6522630232855,5.02437029016278));
#24991=CARTESIAN_POINT('Ctrl Pts',(129.800000548124,-19.5449348183843,4.8588703228705));
#24992=CARTESIAN_POINT('Ctrl Pts',(129.80000051896,-19.4432390432031,4.68973446601173));
#24993=CARTESIAN_POINT('Ctrl Pts',(129.800000489668,-19.3410954998061,4.5198539011183));
#24994=CARTESIAN_POINT('Ctrl Pts',(129.800000488609,-19.2446343708263,4.34630591443198));
#24995=CARTESIAN_POINT('Ctrl Pts',(129.800000499014,-19.1541670592512,4.16971083259214));
#24996=CARTESIAN_POINT('Ctrl Pts',(129.800000509398,-19.0638896851603,3.99348651478835));
#24997=CARTESIAN_POINT('Ctrl Pts',(129.800000530948,-18.9795812093161,3.81422846757693));
#24998=CARTESIAN_POINT('Ctrl Pts',(129.800000547183,-18.9015037433399,3.63257374586257));
#24999=CARTESIAN_POINT('Ctrl Pts',(129.800000561419,-18.833039824863,3.47328586551307));
#25000=CARTESIAN_POINT('Ctrl Pts',(129.800000571427,-18.7693663510026,3.31215571629702));
#25001=CARTESIAN_POINT('Ctrl Pts',(129.800000568889,-18.7106279760856,3.14962062448637));
#25002=CARTESIAN_POINT('Ctrl Pts',(129.800000566223,-18.6489651348561,2.97899323524206));
#25003=CARTESIAN_POINT('Ctrl Pts',(129.800000549463,-18.5927410214724,2.80681784335779));
#25004=CARTESIAN_POINT('Ctrl Pts',(129.800000516707,-18.5418874848769,2.63360653112291));
#25005=CARTESIAN_POINT('Ctrl Pts',(129.800000479892,-18.4847332758541,2.4389346123663));
#25006=CARTESIAN_POINT('Ctrl Pts',(129.800000403875,-18.434039176132,2.24191692469441));
#25007=CARTESIAN_POINT('Ctrl Pts',(129.800000328221,-18.3898852098275,2.04317779165805));
#25008=CARTESIAN_POINT('Ctrl Pts',(129.800000250561,-18.3445597096759,1.83916552824253));
#25009=CARTESIAN_POINT('Ctrl Pts',(129.800000174245,-18.3061261971566,1.63333977252411));
#25010=CARTESIAN_POINT('Ctrl Pts',(129.800000119979,-18.2746223705535,1.42640102500768));
#25011=CARTESIAN_POINT('Ctrl Pts',(129.800000064988,-18.2426979670519,1.21669963986911));
#25012=CARTESIAN_POINT('Ctrl Pts',(129.800000032225,-18.2178895579574,1.00585598704665));
#25013=CARTESIAN_POINT('Ctrl Pts',(129.800000016489,-18.2001851255581,0.794615559855742));
#25014=CARTESIAN_POINT('Ctrl Pts',(129.800000000526,-18.182223881897,0.580310989210295));
#25015=CARTESIAN_POINT('Ctrl Pts',(129.800000000194,-18.1715742168204,0.365598745704213));
#25016=CARTESIAN_POINT('Ctrl Pts',(129.80000000003,-18.1681706704168,0.151263981325619));
#25017=CARTESIAN_POINT('Ctrl Pts',(129.799999999991,-18.1673696146262,0.100818333234996));
#25018=CARTESIAN_POINT('Ctrl Pts',(129.8,-18.1669697220177,0.050393597992155));
#25019=CARTESIAN_POINT('Ctrl Pts',(129.8,-18.1669697220177,4.53337703798322E-15));
#25020=CARTESIAN_POINT('Origin',(131.8,-18.1669697220177,4.71844785465692E-15));
#25021=CARTESIAN_POINT('Ctrl Pts',(132.432701479047,-28.,-7.23809523809524));
#25022=CARTESIAN_POINT('Ctrl Pts',(132.432701479047,-26.8009816752416,-7.23809523809524));
#25023=CARTESIAN_POINT('Ctrl Pts',(132.26645359153,-25.0007435382869,-6.85507520667426));
#25024=CARTESIAN_POINT('Ctrl Pts',(131.781589365556,-22.5441190611736,-5.46533378045002));
#25025=CARTESIAN_POINT('Ctrl Pts',(131.341321658826,-21.023111279012,-3.82480829163835));
#25026=CARTESIAN_POINT('Ctrl Pts',(131.053974250738,-20.1562205092697,-1.73171255809164));
#25027=CARTESIAN_POINT('Ctrl Pts',(131.,-20.,-0.573980617392535));
#25028=CARTESIAN_POINT('Ctrl Pts',(131.,-20.,3.98986399474666E-15));
#25029=CARTESIAN_POINT('Ctrl Pts',(132.090706623172,-28.,-7.12404769267737));
#25030=CARTESIAN_POINT('Ctrl Pts',(132.090706623172,-26.8143903768838,-7.12404769267737));
#25031=CARTESIAN_POINT('Ctrl Pts',(131.929220024804,-25.032371992221,-6.78231349114718));
#25032=CARTESIAN_POINT('Ctrl Pts',(131.480860519403,-22.5478129793514,-5.47666315644241));
#25033=CARTESIAN_POINT('Ctrl Pts',(131.091394358315,-20.9713812405232,-3.8623482138183));
#25034=CARTESIAN_POINT('Ctrl Pts',(130.843813934656,-20.0728982691064,-1.75132320290942));
#25035=CARTESIAN_POINT('Ctrl Pts',(130.797619582017,-19.9116739443255,-0.580551775628326));
#25036=CARTESIAN_POINT('Ctrl Pts',(130.797619582017,-19.9116739443255,4.00881225491749E-15));
#25037=CARTESIAN_POINT('Ctrl Pts',(131.345671187872,-28.,-7.08620083875834));
#25038=CARTESIAN_POINT('Ctrl Pts',(131.345671187872,-26.818798622422,-7.08620083875834));
#25039=CARTESIAN_POINT('Ctrl Pts',(131.217018773873,-25.0379511743519,-6.80862333715474));
#25040=CARTESIAN_POINT('Ctrl Pts',(130.885776810888,-22.4629637836557,-5.6034495189424));
#25041=CARTESIAN_POINT('Ctrl Pts',(130.616860535725,-20.7817899251647,-3.98402852846389));
#25042=CARTESIAN_POINT('Ctrl Pts',(130.453039217185,-19.8354212605226,-1.80583906043873));
#25043=CARTESIAN_POINT('Ctrl Pts',(130.4226711313,-19.6673356519921,-0.598748896272704));
#25044=CARTESIAN_POINT('Ctrl Pts',(130.4226711313,-19.6673356519921,4.13658632801098E-15));
#25045=CARTESIAN_POINT('Ctrl Pts',(130.187837825679,-28.,-7.70051010024203));
#25046=CARTESIAN_POINT('Ctrl Pts',(130.187837825679,-26.7469538948703,-7.70051010024203));
#25047=CARTESIAN_POINT('Ctrl Pts',(130.149022478866,-24.8470535326785,-7.43645293090163));
#25048=CARTESIAN_POINT('Ctrl Pts',(130.056596105886,-22.0269455952546,-6.14421728129872));
#25049=CARTESIAN_POINT('Ctrl Pts',(129.987591470929,-20.1995226886221,-4.33137686974819));
#25050=CARTESIAN_POINT('Ctrl Pts',(129.947669172038,-19.2197159043987,-1.94474772386544));
#25051=CARTESIAN_POINT('Ctrl Pts',(129.94039562733,-19.0495950039424,-0.644745782382747));
#25052=CARTESIAN_POINT('Ctrl Pts',(129.94039562733,-19.0495950039424,4.64941528572959E-15));
#25053=CARTESIAN_POINT('Ctrl Pts',(129.8,-28.,-8.59461511716011));
#25054=CARTESIAN_POINT('Ctrl Pts',(129.8,-26.6424865111779,-8.59461511716011));
#25055=CARTESIAN_POINT('Ctrl Pts',(129.799352153585,-24.5784055571512,-8.26261724319198));
#25056=CARTESIAN_POINT('Ctrl Pts',(129.800907688529,-21.5374980704997,-6.72536392331271));
#25057=CARTESIAN_POINT('Ctrl Pts',(129.800369726049,-19.6351532628125,-4.65866809558641));
#25058=CARTESIAN_POINT('Ctrl Pts',(129.800544621058,-18.6635321684884,-2.06928349402084));
#25059=CARTESIAN_POINT('Ctrl Pts',(129.8,-18.4981924307969,-0.685799821188036));
#25060=CARTESIAN_POINT('Ctrl Pts',(129.8,-18.4981924307969,5.22539942166253E-15));
#25061=CARTESIAN_POINT('Ctrl Pts',(129.8,-28.,-9.13537983414593));
#25062=CARTESIAN_POINT('Ctrl Pts',(129.8,-26.5790536024284,-9.13537983414592));
#25063=CARTESIAN_POINT('Ctrl Pts',(129.8,-24.4156431485582,-8.76163646629594));
#25064=CARTESIAN_POINT('Ctrl Pts',(129.8,-21.242356094889,-7.07450440768049));
#25065=CARTESIAN_POINT('Ctrl Pts',(129.8,-19.2957674742455,-4.85510844114429));
#25066=CARTESIAN_POINT('Ctrl Pts',(129.8,-18.3293873963884,-2.14384019547752));
#25067=CARTESIAN_POINT('Ctrl Pts',(129.8,-18.1669697220177,-0.710473198785783));
#25068=CARTESIAN_POINT('Ctrl Pts',(129.8,-18.1669697220177,5.60575888572018E-15));
#25069=CARTESIAN_POINT('Ctrl Pts',(129.8,-18.1669697220177,5.60575888572018E-15));
#25070=CARTESIAN_POINT('Ctrl Pts',(129.8,-18.1669697220177,-0.710473198785783));
#25071=CARTESIAN_POINT('Ctrl Pts',(129.8,-18.3293873963884,-2.14384019547752));
#25072=CARTESIAN_POINT('Ctrl Pts',(129.8,-19.2957674742455,-4.85510844114429));
#25073=CARTESIAN_POINT('Ctrl Pts',(129.8,-21.242356094889,-7.07450440768049));
#25074=CARTESIAN_POINT('Ctrl Pts',(129.8,-24.4156431485582,-8.76163646629594));
#25075=CARTESIAN_POINT('Ctrl Pts',(129.8,-26.5790536024284,-9.13537983414592));
#25076=CARTESIAN_POINT('Ctrl Pts',(129.8,-28.,-9.13537983414593));
#25077=CARTESIAN_POINT('Origin',(129.8,16.6,0.));
#25078=CARTESIAN_POINT('',(129.8,-16.6,-2.03291368658461E-15));
#25079=CARTESIAN_POINT('Origin',(129.8,0.,0.));
#25080=CARTESIAN_POINT('Origin',(160.,-32.,-32.));
#25081=CARTESIAN_POINT('',(160.,-41.8103991881704,-58.2251037704095));
#25082=CARTESIAN_POINT('Origin',(160.,-32.,-32.));
#25083=CARTESIAN_POINT('',(162.,-42.9545404089977,-55.579610777696));
#25084=CARTESIAN_POINT('Ctrl Pts',(162.,-42.9545404089977,-55.579610777696));
#25085=CARTESIAN_POINT('Ctrl Pts',(162.,-43.0271281214294,-55.7530160455202));
#25086=CARTESIAN_POINT('Ctrl Pts',(161.973573983972,-43.0736878043345,-55.9328516982979));
#25087=CARTESIAN_POINT('Ctrl Pts',(161.868475569496,-43.1203520588171,-56.3211207154451));
#25088=CARTESIAN_POINT('Ctrl Pts',(161.784372185244,-43.1115565863127,-56.522998392291));
#25089=CARTESIAN_POINT('Ctrl Pts',(161.547930236135,-43.0311442891192,-56.9623937955494));
#25090=CARTESIAN_POINT('Ctrl Pts',(161.383204155006,-42.9404796484396,-57.1887874178576));
#25091=CARTESIAN_POINT('Ctrl Pts',(161.02783774489,-42.7034153293614,-57.5819163169907));
#25092=CARTESIAN_POINT('Ctrl Pts',(160.835005517045,-42.5553839363861,-57.7505434494708));
#25093=CARTESIAN_POINT('Ctrl Pts',(160.431659980245,-42.2166967899328,-58.0327463433367));
#25094=CARTESIAN_POINT('Ctrl Pts',(160.218422653963,-42.0224470249448,-58.1450131095542));
#25095=CARTESIAN_POINT('Ctrl Pts',(160.004130040426,-41.8144122444641,-58.2235988717642));
#25096=CARTESIAN_POINT('Ctrl Pts',(160.002065019734,-41.812406319229,-58.2243529342229));
#25097=CARTESIAN_POINT('Ctrl Pts',(160.,-41.8103991881673,-58.2251037704106));
#25098=CARTESIAN_POINT('Origin',(162.,-32.,-32.));
#25099=CARTESIAN_POINT('Origin',(162.,-45.,-45.));
#25100=CARTESIAN_POINT('',(162.,-41.7580469908461,-54.4599017271026));
#25101=CARTESIAN_POINT('Origin',(162.,-41.1096563890154,-56.3518820725231));
#25102=CARTESIAN_POINT('Origin',(162.,-45.,-45.));
#25103=CARTESIAN_POINT('',(162.,-45.,-38.5));
#25104=CARTESIAN_POINT('Origin',(162.,-45.,-45.));
#25105=CARTESIAN_POINT('Origin',(160.,-32.,32.));
#25106=CARTESIAN_POINT('',(160.,-58.153393661244,42.));
#25107=CARTESIAN_POINT('',(162.,-55.5753783097334,42.9636461796681));
#25108=CARTESIAN_POINT('Ctrl Pts',(162.,-55.5753783097334,42.9636461796681));
#25109=CARTESIAN_POINT('Ctrl Pts',(162.,-55.6734613307539,43.0052418396728));
#25110=CARTESIAN_POINT('Ctrl Pts',(161.991497625313,-55.774572253448,43.0388739116958));
#25111=CARTESIAN_POINT('Ctrl Pts',(161.943944452234,-56.0679790385642,43.1111756115417));
#25112=CARTESIAN_POINT('Ctrl Pts',(161.886488114777,-56.257458287516,43.1282512264031));
#25113=CARTESIAN_POINT('Ctrl Pts',(161.713845454435,-56.6687617144824,43.1110662555161));
#25114=CARTESIAN_POINT('Ctrl Pts',(161.589392283786,-56.8825885356347,43.0628215369467));
#25115=CARTESIAN_POINT('Ctrl Pts',(161.260245422218,-57.3380017544373,42.8875266559234));
#25116=CARTESIAN_POINT('Ctrl Pts',(161.041527470277,-57.5632038812665,42.7369834456557));
#25117=CARTESIAN_POINT('Ctrl Pts',(160.689312921863,-57.8437159943844,42.4663518758168));
#25118=CARTESIAN_POINT('Ctrl Pts',(160.563162669358,-57.9294120770491,42.3637163836509));
#25119=CARTESIAN_POINT('Ctrl Pts',(160.344401686438,-58.0513270922311,42.1875089376441));
#25120=CARTESIAN_POINT('Ctrl Pts',(160.263056078934,-58.0887104512742,42.1229599723016));
#25121=CARTESIAN_POINT('Ctrl Pts',(160.155587043591,-58.1276579654234,42.0513407387634));
#25122=CARTESIAN_POINT('Ctrl Pts',(160.11788316197,-58.1386506822474,42.0296954878548));
#25123=CARTESIAN_POINT('Ctrl Pts',(160.053942941167,-58.1506706840953,42.0056317234313));
#25124=CARTESIAN_POINT('Ctrl Pts',(160.028265792271,-58.1531925095842,42.0004118971055));
#25125=CARTESIAN_POINT('Ctrl Pts',(160.002031326826,-58.1533898527096,42.0000077985377));
#25126=CARTESIAN_POINT('Ctrl Pts',(160.001014693341,-58.1533936622468,41.9999999973774));
#25127=CARTESIAN_POINT('Ctrl Pts',(160.,-58.1533936622468,41.9999999973774));
#25128=CARTESIAN_POINT('',(162.,-42.9545404089977,55.579610777696));
#25129=CARTESIAN_POINT('Origin',(162.,-32.,32.));
#25130=CARTESIAN_POINT('',(160.,-41.8103991881704,58.2251037704095));
#25131=CARTESIAN_POINT('Ctrl Pts',(160.,-41.8103991881673,58.2251037704106));
#25132=CARTESIAN_POINT('Ctrl Pts',(160.002065019732,-41.8124063192265,58.2243529342238));
#25133=CARTESIAN_POINT('Ctrl Pts',(160.004130040429,-41.8144122444637,58.2235988717643));
#25134=CARTESIAN_POINT('Ctrl Pts',(160.218422653916,-42.022447024985,58.1450131095393));
#25135=CARTESIAN_POINT('Ctrl Pts',(160.431659980247,-42.2166967899343,58.0327463433355));
#25136=CARTESIAN_POINT('Ctrl Pts',(160.835005517045,-42.5553839363861,57.7505434494708));
#25137=CARTESIAN_POINT('Ctrl Pts',(161.02783774489,-42.7034153293614,57.5819163169908));
#25138=CARTESIAN_POINT('Ctrl Pts',(161.383204155006,-42.9404796484396,57.1887874178575));
#25139=CARTESIAN_POINT('Ctrl Pts',(161.547930236135,-43.0311442891192,56.9623937955494));
#25140=CARTESIAN_POINT('Ctrl Pts',(161.784372185244,-43.1115565863127,56.5229983922909));
#25141=CARTESIAN_POINT('Ctrl Pts',(161.868475569496,-43.1203520588171,56.3211207154451));
#25142=CARTESIAN_POINT('Ctrl Pts',(161.973573983972,-43.0736878043345,55.9328516982979));
#25143=CARTESIAN_POINT('Ctrl Pts',(162.,-43.0271281214294,55.7530160455202));
#25144=CARTESIAN_POINT('Ctrl Pts',(162.,-42.9545404089977,55.579610777696));
#25145=CARTESIAN_POINT('Origin',(160.,-32.,32.));
#25146=CARTESIAN_POINT('Origin',(125.8,-32.,32.));
#25147=CARTESIAN_POINT('',(173.,-41.8103991881704,58.2251037704095));
#25148=CARTESIAN_POINT('',(125.8,-41.8103991881704,58.2251037704095));
#25149=CARTESIAN_POINT('',(173.,-32.,60.));
#25150=CARTESIAN_POINT('Origin',(173.,-32.,32.));
#25151=CARTESIAN_POINT('',(127.8,-32.,60.));
#25152=CARTESIAN_POINT('',(125.8,-32.,60.));
#25153=CARTESIAN_POINT('Origin',(127.8,-32.,32.));
#25154=CARTESIAN_POINT('',(125.8,-58.153393661244,42.));
#25155=CARTESIAN_POINT('Origin',(160.,32.,-32.));
#25156=CARTESIAN_POINT('',(160.,58.2251037704095,-41.8103991881704));
#25157=CARTESIAN_POINT('',(162.,55.579610777696,-42.9545404089977));
#25158=CARTESIAN_POINT('Ctrl Pts',(162.,55.579610777696,-42.9545404089977));
#25159=CARTESIAN_POINT('Ctrl Pts',(162.,55.7530160455202,-43.0271281214294));
#25160=CARTESIAN_POINT('Ctrl Pts',(161.973573983972,55.9328516982979,-43.0736878043345));
#25161=CARTESIAN_POINT('Ctrl Pts',(161.868475569496,56.3211207154452,-43.1203520588171));
#25162=CARTESIAN_POINT('Ctrl Pts',(161.784372185244,56.522998392291,-43.1115565863127));
#25163=CARTESIAN_POINT('Ctrl Pts',(161.547930236135,56.9623937955493,-43.0311442891192));
#25164=CARTESIAN_POINT('Ctrl Pts',(161.383204155006,57.1887874178575,-42.9404796484396));
#25165=CARTESIAN_POINT('Ctrl Pts',(161.027837744889,57.5819163169916,-42.7034153293609));
#25166=CARTESIAN_POINT('Ctrl Pts',(160.835005517043,57.7505434494722,-42.5553839363849));
#25167=CARTESIAN_POINT('Ctrl Pts',(160.431659980243,58.0327463433376,-42.2166967899313));
#25168=CARTESIAN_POINT('Ctrl Pts',(160.218422653911,58.1450131095417,-42.0224470249804));
#25169=CARTESIAN_POINT('Ctrl Pts',(160.004130040426,58.2235988717657,-41.8144122444601));
#25170=CARTESIAN_POINT('Ctrl Pts',(160.00206501973,58.2243529342232,-41.8124063192281));
#25171=CARTESIAN_POINT('Ctrl Pts',(160.,58.2251037704095,-41.8103991881704));
#25172=CARTESIAN_POINT('',(162.,42.9545404089977,-55.579610777696));
#25173=CARTESIAN_POINT('Origin',(162.,32.,-32.));
#25174=CARTESIAN_POINT('',(160.,41.8103991881704,-58.2251037704095));
#25175=CARTESIAN_POINT('Ctrl Pts',(160.,41.8103991881704,-58.2251037704095));
#25176=CARTESIAN_POINT('Ctrl Pts',(160.002065019731,41.8124063192286,-58.224352934223));
#25177=CARTESIAN_POINT('Ctrl Pts',(160.004130040425,41.8144122444596,-58.2235988717659));
#25178=CARTESIAN_POINT('Ctrl Pts',(160.218422653911,42.0224470249804,-58.1450131095417));
#25179=CARTESIAN_POINT('Ctrl Pts',(160.431659980243,42.2166967899313,-58.0327463433376));
#25180=CARTESIAN_POINT('Ctrl Pts',(160.835005517043,42.5553839363849,-57.7505434494722));
#25181=CARTESIAN_POINT('Ctrl Pts',(161.027837744889,42.7034153293609,-57.5819163169915));
#25182=CARTESIAN_POINT('Ctrl Pts',(161.383204155006,42.9404796484396,-57.1887874178575));
#25183=CARTESIAN_POINT('Ctrl Pts',(161.547930236135,43.0311442891192,-56.9623937955494));
#25184=CARTESIAN_POINT('Ctrl Pts',(161.784372185244,43.1115565863127,-56.522998392291));
#25185=CARTESIAN_POINT('Ctrl Pts',(161.868475569496,43.1203520588171,-56.3211207154451));
#25186=CARTESIAN_POINT('Ctrl Pts',(161.973573983972,43.0736878043345,-55.9328516982979));
#25187=CARTESIAN_POINT('Ctrl Pts',(162.,43.0271281214294,-55.7530160455202));
#25188=CARTESIAN_POINT('Ctrl Pts',(162.,42.9545404089977,-55.579610777696));
#25189=CARTESIAN_POINT('Origin',(160.,32.,-32.));
#25190=CARTESIAN_POINT('Origin',(162.,45.,-45.));
#25191=CARTESIAN_POINT('',(162.,54.4599017271026,-41.7580469908461));
#25192=CARTESIAN_POINT('Origin',(162.,56.3518820725231,-41.1096563890154));
#25193=CARTESIAN_POINT('',(162.,41.7580469908461,-54.4599017271026));
#25194=CARTESIAN_POINT('Origin',(162.,45.,-45.));
#25195=CARTESIAN_POINT('Origin',(162.,41.1096563890154,-56.3518820725231));
#25196=CARTESIAN_POINT('',(162.,45.,-38.5));
#25197=CARTESIAN_POINT('Origin',(162.,45.,-45.));
#25198=CARTESIAN_POINT('Origin',(160.,32.,32.));
#25199=CARTESIAN_POINT('',(160.,41.8103991881704,58.2251037704095));
#25200=CARTESIAN_POINT('',(162.,42.9545404089977,55.579610777696));
#25201=CARTESIAN_POINT('Ctrl Pts',(162.,42.9545404089977,55.579610777696));
#25202=CARTESIAN_POINT('Ctrl Pts',(162.,43.0271281214294,55.7530160455202));
#25203=CARTESIAN_POINT('Ctrl Pts',(161.973573983972,43.0736878043345,55.9328516982979));
#25204=CARTESIAN_POINT('Ctrl Pts',(161.868475569496,43.1203520588171,56.3211207154451));
#25205=CARTESIAN_POINT('Ctrl Pts',(161.784372185244,43.1115565863127,56.522998392291));
#25206=CARTESIAN_POINT('Ctrl Pts',(161.547930236135,43.0311442891192,56.9623937955494));
#25207=CARTESIAN_POINT('Ctrl Pts',(161.383204155006,42.9404796484396,57.1887874178576));
#25208=CARTESIAN_POINT('Ctrl Pts',(161.027837744889,42.7034153293609,57.5819163169915));
#25209=CARTESIAN_POINT('Ctrl Pts',(160.835005517043,42.5553839363849,57.7505434494722));
#25210=CARTESIAN_POINT('Ctrl Pts',(160.431659980243,42.2166967899312,58.0327463433376));
#25211=CARTESIAN_POINT('Ctrl Pts',(160.218422653911,42.0224470249804,58.1450131095417));
#25212=CARTESIAN_POINT('Ctrl Pts',(160.004130040425,41.8144122444596,58.2235988717659));
#25213=CARTESIAN_POINT('Ctrl Pts',(160.002065019731,41.8124063192286,58.224352934223));
#25214=CARTESIAN_POINT('Ctrl Pts',(160.,41.8103991881704,58.2251037704095));
#25215=CARTESIAN_POINT('',(162.,55.579610777696,42.9545404089977));
#25216=CARTESIAN_POINT('Origin',(162.,32.,32.));
#25217=CARTESIAN_POINT('',(160.,58.2251037704095,41.8103991881704));
#25218=CARTESIAN_POINT('Ctrl Pts',(160.,58.2251037704095,41.8103991881704));
#25219=CARTESIAN_POINT('Ctrl Pts',(160.00206501973,58.2243529342232,41.8124063192281));
#25220=CARTESIAN_POINT('Ctrl Pts',(160.004130040426,58.2235988717657,41.8144122444601));
#25221=CARTESIAN_POINT('Ctrl Pts',(160.218422653911,58.1450131095417,42.0224470249804));
#25222=CARTESIAN_POINT('Ctrl Pts',(160.431659980243,58.0327463433376,42.2166967899313));
#25223=CARTESIAN_POINT('Ctrl Pts',(160.835005517043,57.7505434494722,42.5553839363849));
#25224=CARTESIAN_POINT('Ctrl Pts',(161.027837744889,57.5819163169915,42.7034153293609));
#25225=CARTESIAN_POINT('Ctrl Pts',(161.383204155006,57.1887874178575,42.9404796484396));
#25226=CARTESIAN_POINT('Ctrl Pts',(161.547930236135,56.9623937955494,43.0311442891192));
#25227=CARTESIAN_POINT('Ctrl Pts',(161.784372185244,56.522998392291,43.1115565863127));
#25228=CARTESIAN_POINT('Ctrl Pts',(161.868475569496,56.3211207154451,43.1203520588171));
#25229=CARTESIAN_POINT('Ctrl Pts',(161.973573983972,55.9328516982979,43.0736878043345));
#25230=CARTESIAN_POINT('Ctrl Pts',(162.,55.7530160455202,43.0271281214294));
#25231=CARTESIAN_POINT('Ctrl Pts',(162.,55.579610777696,42.9545404089977));
#25232=CARTESIAN_POINT('Origin',(160.,32.,32.));
#25233=CARTESIAN_POINT('Origin',(162.,45.,45.));
#25234=CARTESIAN_POINT('',(162.,41.7580469908461,54.4599017271026));
#25235=CARTESIAN_POINT('Origin',(162.,41.1096563890154,56.3518820725231));
#25236=CARTESIAN_POINT('',(162.,54.4599017271026,41.7580469908461));
#25237=CARTESIAN_POINT('Origin',(162.,45.,45.));
#25238=CARTESIAN_POINT('Origin',(162.,56.3518820725231,41.1096563890154));
#25239=CARTESIAN_POINT('',(162.,45.,51.5));
#25240=CARTESIAN_POINT('Origin',(162.,45.,45.));
#25241=CARTESIAN_POINT('Origin',(127.8,16.,58.));
#25242=CARTESIAN_POINT('',(127.8,32.,60.));
#25243=CARTESIAN_POINT('Origin',(127.8,32.,58.));
#25244=CARTESIAN_POINT('Origin',(127.8,-32.,58.));
#25245=CARTESIAN_POINT('',(127.8,16.,60.));
#25246=CARTESIAN_POINT('Origin',(127.8,-32.,32.));
#25247=CARTESIAN_POINT('Origin',(127.8,32.,32.));
#25248=CARTESIAN_POINT('Origin',(127.8,32.,32.));
#25249=CARTESIAN_POINT('Origin',(125.8,32.,32.));
#25250=CARTESIAN_POINT('',(173.,58.2251037704095,41.8103991881704));
#25251=CARTESIAN_POINT('',(125.8,58.2251037704095,41.8103991881704));
#25252=CARTESIAN_POINT('Origin',(173.,32.,32.));
#25253=CARTESIAN_POINT('',(125.8,59.9821371592664,33.));
#25254=CARTESIAN_POINT('',(173.,32.,60.));
#25255=CARTESIAN_POINT('',(125.8,32.,60.));
#25256=CARTESIAN_POINT('',(173.,41.8103991881704,58.2251037704095));
#25257=CARTESIAN_POINT('Origin',(173.,32.,32.));
#25258=CARTESIAN_POINT('',(125.8,41.8103991881704,58.2251037704095));
#25259=CARTESIAN_POINT('Origin',(125.8,32.,60.));
#25260=CARTESIAN_POINT('',(173.,16.,60.));
#25261=CARTESIAN_POINT('Origin',(173.,-32.,-32.));
#25262=CARTESIAN_POINT('',(173.,-32.,-60.));
#25263=CARTESIAN_POINT('Origin',(173.,-32.,-58.));
#25264=CARTESIAN_POINT('',(173.,-41.8103991881704,-58.2251037704095));
#25265=CARTESIAN_POINT('Origin',(173.,-41.1096563890154,-56.3518820725231));
#25266=CARTESIAN_POINT('Origin',(173.,-32.,-32.));
#25267=CARTESIAN_POINT('Origin',(173.,-16.,-58.));
#25268=CARTESIAN_POINT('',(173.,32.,-60.));
#25269=CARTESIAN_POINT('Origin',(173.,32.,-58.));
#25270=CARTESIAN_POINT('',(173.,-16.,-60.));
#25271=CARTESIAN_POINT('Origin',(173.,32.,-32.));
#25272=CARTESIAN_POINT('',(173.,41.8103991881704,-58.2251037704095));
#25273=CARTESIAN_POINT('Origin',(173.,41.1096563890154,-56.3518820725231));
#25274=CARTESIAN_POINT('Origin',(173.,32.,-32.));
#25275=CARTESIAN_POINT('Origin',(173.,41.1096563890154,-56.3518820725231));
#25276=CARTESIAN_POINT('',(173.,41.7580469908461,-54.4599017271026));
#25277=CARTESIAN_POINT('Origin',(173.,41.1096563890154,-56.3518820725231));
#25278=CARTESIAN_POINT('Origin',(173.,41.1096563890154,-56.3518820725231));
#25279=CARTESIAN_POINT('Origin',(173.,-41.1096563890154,-56.3518820725231));
#25280=CARTESIAN_POINT('',(173.,-41.7580469908461,-54.4599017271026));
#25281=CARTESIAN_POINT('Origin',(173.,-41.1096563890154,-56.3518820725231));
#25282=CARTESIAN_POINT('Origin',(173.,-41.1096563890154,-56.3518820725231));
#25283=CARTESIAN_POINT('Origin',(173.,45.,-45.));
#25284=CARTESIAN_POINT('',(173.,54.4599017271026,-41.7580469908461));
#25285=CARTESIAN_POINT('Origin',(173.,45.,-45.));
#25286=CARTESIAN_POINT('Origin',(173.,56.3518820725231,-41.1096563890154));
#25287=CARTESIAN_POINT('Origin',(125.8,41.1096563890154,-56.3518820725231));
#25288=CARTESIAN_POINT('',(125.8,41.8103991881704,-58.2251037704095));
#25289=CARTESIAN_POINT('',(125.8,41.7580469908461,-54.4599017271026));
#25290=CARTESIAN_POINT('Origin',(125.8,32.,-32.));
#25291=CARTESIAN_POINT('',(173.,58.2251037704095,-41.8103991881704));
#25292=CARTESIAN_POINT('Origin',(173.,32.,-32.));
#25293=CARTESIAN_POINT('',(125.8,58.2251037704095,-41.8103991881704));
#25294=CARTESIAN_POINT('',(125.8,32.,-60.));
#25295=CARTESIAN_POINT('Origin',(125.8,-32.,-60.));
#25296=CARTESIAN_POINT('',(125.8,-32.,-60.));
#25297=CARTESIAN_POINT('Origin',(125.8,-32.,-32.));
#25298=CARTESIAN_POINT('',(125.8,-41.8103991881704,-58.2251037704095));
#25299=CARTESIAN_POINT('Origin',(173.,-30.,40.));
#25300=CARTESIAN_POINT('',(173.,-58.153393661244,42.));
#25301=CARTESIAN_POINT('Ctrl Pts',(173.,-58.1533936609661,42.));
#25302=CARTESIAN_POINT('Ctrl Pts',(173.167046229782,-58.1533936609661,42.));
#25303=CARTESIAN_POINT('Ctrl Pts',(173.335981739515,-58.164172163974,41.9788285866254));
#25304=CARTESIAN_POINT('Ctrl Pts',(173.663743266442,-58.2018772085049,41.8942257523252));
#25305=CARTESIAN_POINT('Ctrl Pts',(173.822610223296,-58.2285507903109,41.8308404000117));
#25306=CARTESIAN_POINT('Ctrl Pts',(174.118673603566,-58.2827371839977,41.6665038929614));
#25307=CARTESIAN_POINT('Ctrl Pts',(174.256201391015,-58.3101344177017,41.5653968322566));
#25308=CARTESIAN_POINT('Ctrl Pts',(174.420873583764,-58.3360427437949,41.4087347797136));
#25309=CARTESIAN_POINT('Ctrl Pts',(174.461424720572,-58.3417521272735,41.3666159110033));
#25310=CARTESIAN_POINT('Ctrl Pts',(174.499999999851,-58.3461592103039,41.3228756557013));
#25311=CARTESIAN_POINT('',(173.,-30.,42.));
#25312=CARTESIAN_POINT('Origin',(150.4,-60.,42.));
#25313=CARTESIAN_POINT('',(125.8,-58.153393661244,42.));
#25314=CARTESIAN_POINT('Origin',(173.,26.5,-31.));
#25315=CARTESIAN_POINT('Origin',(173.,64.,-31.));
#25316=CARTESIAN_POINT('Ctrl Pts',(173.,59.9821371592664,-33.));
#25317=CARTESIAN_POINT('Ctrl Pts',(173.100941314786,59.9821371592664,-33.));
#25318=CARTESIAN_POINT('Ctrl Pts',(173.20122849925,59.9747656314413,-32.9923574576679));
#25319=CARTESIAN_POINT('Ctrl Pts',(173.448747816884,59.9385021348617,-32.9548041970754));
#25320=CARTESIAN_POINT('Ctrl Pts',(173.591032753534,59.9010691778161,-32.9160577581803));
#25321=CARTESIAN_POINT('Ctrl Pts',(173.946053385859,59.7672434939636,-32.7780158331181));
#25322=CARTESIAN_POINT('Ctrl Pts',(174.150696148371,59.6459583395498,-32.6532332234613));
#25323=CARTESIAN_POINT('Ctrl Pts',(174.50787466907,59.3337989076212,-32.3354122100756));
#25324=CARTESIAN_POINT('Ctrl Pts',(174.647363992728,59.1545342172527,-32.1543180026668));
#25325=CARTESIAN_POINT('Ctrl Pts',(174.914204977564,58.6701679370831,-31.6705622009276));
#25326=CARTESIAN_POINT('Ctrl Pts',(174.999017799315,58.3344432492769,-31.3404083795624));
#25327=CARTESIAN_POINT('Ctrl Pts',(174.999997177196,57.9847942903201,-31.0038801897555));
#25328=CARTESIAN_POINT('Ctrl Pts',(175.,57.9827782576495,-31.0019400355805));
#25329=CARTESIAN_POINT('Ctrl Pts',(175.,57.9807621135332,-31.));
#25330=CARTESIAN_POINT('Origin',(173.,64.,-31.));
#25331=CARTESIAN_POINT('Origin',(173.,-45.,-45.));
#25332=CARTESIAN_POINT('Origin',(173.,-45.,-45.));
#25333=CARTESIAN_POINT('Origin',(125.8,-41.1096563890154,-56.3518820725231));
#25334=CARTESIAN_POINT('',(125.8,-41.7580469908461,-54.4599017271026));
#25335=CARTESIAN_POINT('Origin',(125.8,-56.3562342901464,41.1223792414288));
#25336=CARTESIAN_POINT('',(162.,-54.463528575122,41.7686493678573));
#25337=CARTESIAN_POINT('',(125.8,-54.463528575122,41.7686493678573));
#25338=CARTESIAN_POINT('Origin',(162.,-56.3562342901464,41.1223792414288));
#25339=CARTESIAN_POINT('Origin',(175.,-45.,45.));
#25340=CARTESIAN_POINT('',(162.,-41.7580469908461,54.4599017271026));
#25341=CARTESIAN_POINT('',(125.8,-41.7580469908461,54.4599017271026));
#25342=CARTESIAN_POINT('Origin',(162.,-45.,45.));
#25343=CARTESIAN_POINT('Origin',(173.,56.3518820725231,41.1096563890154));
#25344=CARTESIAN_POINT('',(173.,54.4599017271026,41.7580469908461));
#25345=CARTESIAN_POINT('Origin',(173.,56.3518820725231,41.1096563890154));
#25346=CARTESIAN_POINT('Origin',(173.,56.3518820725231,41.1096563890154));
#25347=CARTESIAN_POINT('Origin',(173.,56.3518820725231,41.1096563890154));
#25348=CARTESIAN_POINT('Origin',(173.,41.1096563890154,56.3518820725231));
#25349=CARTESIAN_POINT('',(173.,41.7580469908461,54.4599017271026));
#25350=CARTESIAN_POINT('Origin',(173.,41.1096563890154,56.3518820725231));
#25351=CARTESIAN_POINT('Origin',(173.,41.1096563890154,56.3518820725231));
#25352=CARTESIAN_POINT('Origin',(173.,41.1096563890154,56.3518820725231));
#25353=CARTESIAN_POINT('Origin',(173.,-41.1096563890154,56.3518820725231));
#25354=CARTESIAN_POINT('Origin',(173.,-41.1096563890154,56.3518820725231));
#25355=CARTESIAN_POINT('Origin',(173.,-41.1096563890154,56.3518820725231));
#25356=CARTESIAN_POINT('Origin',(173.,32.,32.));
#25357=CARTESIAN_POINT('Origin',(173.,32.,58.));
#25358=CARTESIAN_POINT('Origin',(173.,16.,58.));
#25359=CARTESIAN_POINT('Origin',(173.,-32.,58.));
#25360=CARTESIAN_POINT('Origin',(173.,-32.,32.));
#25361=CARTESIAN_POINT('Origin',(125.8,-41.1096563890154,56.3518820725231));
#25362=CARTESIAN_POINT('Origin',(162.,-41.1096563890154,56.3518820725231));
#25363=CARTESIAN_POINT('Origin',(173.,45.,45.));
#25364=CARTESIAN_POINT('Origin',(173.,45.,45.));
#25365=CARTESIAN_POINT('Origin',(125.8,41.1096563890154,56.3518820725231));
#25366=CARTESIAN_POINT('',(125.8,41.7580469908461,54.4599017271026));
#25367=CARTESIAN_POINT('Origin',(173.,32.,32.));
#25368=CARTESIAN_POINT('Origin',(125.8,56.3518820725231,41.1096563890154));
#25369=CARTESIAN_POINT('',(125.8,54.4599017271026,41.7580469908461));
#25370=CARTESIAN_POINT('Origin',(175.,45.,45.));
#25371=CARTESIAN_POINT('Origin',(173.,56.3518820725231,-41.1096563890154));
#25372=CARTESIAN_POINT('Origin',(173.,56.3518820725231,-41.1096563890154));
#25373=CARTESIAN_POINT('Origin',(173.,56.3518820725231,-41.1096563890154));
#25374=CARTESIAN_POINT('Origin',(173.,32.,-32.));
#25375=CARTESIAN_POINT('Origin',(125.8,56.3518820725231,-41.1096563890154));
#25376=CARTESIAN_POINT('',(125.8,54.4599017271026,-41.7580469908461));
#25377=CARTESIAN_POINT('Origin',(162.,45.,-45.));
#25378=CARTESIAN_POINT('',(162.,45.,-38.5));
#25379=CARTESIAN_POINT('Origin',(162.,-45.,45.));
#25380=CARTESIAN_POINT('',(162.,-45.,51.5));
#25381=CARTESIAN_POINT('Origin',(162.,-45.,45.));
#25382=CARTESIAN_POINT('',(162.,-45.,51.5));
#25383=CARTESIAN_POINT('Origin',(162.,45.,45.));
#25384=CARTESIAN_POINT('',(162.,45.,51.5));
#25385=CARTESIAN_POINT('Origin',(162.,-45.,-45.));
#25386=CARTESIAN_POINT('',(162.,-45.,-38.5));
#25387=CARTESIAN_POINT('Origin',(175.,45.,-45.));
#25388=CARTESIAN_POINT('Origin',(162.,-45.,45.));
#25389=CARTESIAN_POINT('Origin',(175.,-45.,-45.));
#25390=CARTESIAN_POINT('Origin',(132.15,-62.,34.95));
#25391=CARTESIAN_POINT('Origin',(167.85,-62.,-34.95));
#25392=CARTESIAN_POINT('Origin',(167.85,-62.,34.95));
#25393=CARTESIAN_POINT('Origin',(132.15,-62.,-34.95));
#25394=CARTESIAN_POINT('Origin',(150.,-20.,0.));
#25395=CARTESIAN_POINT('Origin',(138.1,49.,25.4));
#25396=CARTESIAN_POINT('Origin',(161.9,49.,-25.4));
#25397=CARTESIAN_POINT('Origin',(161.9,49.,25.4));
#25398=CARTESIAN_POINT('Origin',(138.1,49.,-25.4));
#25399=CARTESIAN_POINT('Origin',(150.,20.,0.));
#25400=CARTESIAN_POINT('Origin',(128.25,0.,0.));
#25401=CARTESIAN_POINT('',(130.8,-16.6,-2.03291368658461E-15));
#25402=CARTESIAN_POINT('',(128.25,-16.6,-2.03291368658461E-15));
#25403=CARTESIAN_POINT('Origin',(130.8,0.,0.));
#25404=CARTESIAN_POINT('Origin',(130.8,16.505,0.));
#25405=CARTESIAN_POINT('',(130.8,-16.505,-2.02127954199271E-15));
#25406=CARTESIAN_POINT('Origin',(130.8,0.,0.));
#25407=CARTESIAN_POINT('Origin',(140.8,0.,0.));
#25408=CARTESIAN_POINT('',(140.8,-16.505,-2.02127954199271E-15));
#25409=CARTESIAN_POINT('Origin',(154.8,0.,0.));
#25410=CARTESIAN_POINT('Origin',(150.4,53.,33.));
#25411=CARTESIAN_POINT('',(0.,0.,0.));
#25412=CARTESIAN_POINT('Origin',(16.25,-24.25,-24.5));
#25413=CARTESIAN_POINT('',(16.,-24.,-41.569219381653));
#25414=CARTESIAN_POINT('',(16.5,-24.5,-41.2765066351308));
#25415=CARTESIAN_POINT('Origin',(-8.0000000000001,0.,0.));
#25416=CARTESIAN_POINT('',(16.5,-24.5,41.2765066351308));
#25417=CARTESIAN_POINT('',(16.5,-24.5,-24.5));
#25418=CARTESIAN_POINT('',(16.,-24.,41.569219381653));
#25419=CARTESIAN_POINT('Origin',(-8.0000000000001,0.,0.));
#25420=CARTESIAN_POINT('',(16.,-24.,-24.5));
#25421=CARTESIAN_POINT('Origin',(34.9605325577062,-24.5,0.));
#25422=CARTESIAN_POINT('',(50.8858188853231,-24.5,-41.2765066351308));
#25423=CARTESIAN_POINT('',(42.5,-24.5,-41.2765066351308));
#25424=CARTESIAN_POINT('',(24.0627188904386,-24.5,41.2765066351308));
#25425=CARTESIAN_POINT('',(29.418817527239,-24.5,24.7921300371634));
#25426=CARTESIAN_POINT('',(42.5,-24.5,41.2765066351308));
#25427=CARTESIAN_POINT('Origin',(42.5,0.,0.));
#25428=CARTESIAN_POINT('',(16.,24.,-41.569219381653));
#25429=CARTESIAN_POINT('Origin',(16.,0.,0.));
#25430=CARTESIAN_POINT('',(16.5,24.5,-41.2765066351308));
#25431=CARTESIAN_POINT('Origin',(-8.0000000000001,0.,0.));
#25432=CARTESIAN_POINT('',(50.8858188853231,24.5,-41.2765066351308));
#25433=CARTESIAN_POINT('',(42.5,24.5,-41.2765066351308));
#25434=CARTESIAN_POINT('',(51.5066581341257,24.,-41.569219381653));
#25435=CARTESIAN_POINT('Origin',(63.2350933817184,0.,0.));
#25436=CARTESIAN_POINT('',(51.5066581341257,-24.,-41.569219381653));
#25437=CARTESIAN_POINT('Origin',(38.,0.,0.));
#25438=CARTESIAN_POINT('Origin',(63.2350933817184,0.,0.));
#25439=CARTESIAN_POINT('Origin',(29.6565816563128,-24.25,24.8693842857571));
#25440=CARTESIAN_POINT('',(24.4933418658742,-24.,41.569219381653));
#25441=CARTESIAN_POINT('Origin',(63.2350933817184,0.,0.));
#25442=CARTESIAN_POINT('',(29.8943457853866,-24.,24.9466385343509));
#25443=CARTESIAN_POINT('Origin',(22.0789348845876,0.,49.));
#25444=CARTESIAN_POINT('',(24.4933418658742,24.,41.569219381653));
#25445=CARTESIAN_POINT('',(29.8943457853866,24.,24.9466385343509));
#25446=CARTESIAN_POINT('Origin',(38.,0.,0.));
#25447=CARTESIAN_POINT('',(38.,-20.,-4.83914384121483E-15));
#25448=CARTESIAN_POINT('Origin',(38.,0.,0.));
#25449=CARTESIAN_POINT('Origin',(16.25,24.25,-24.5));
#25450=CARTESIAN_POINT('',(16.,24.,41.569219381653));
#25451=CARTESIAN_POINT('',(16.5,24.5,41.2765066351308));
#25452=CARTESIAN_POINT('Origin',(-8.0000000000001,0.,0.));
#25453=CARTESIAN_POINT('',(16.5,24.5,-24.5));
#25454=CARTESIAN_POINT('',(16.,24.,-24.5));
#25455=CARTESIAN_POINT('Origin',(16.,0.,-49.));
#25456=CARTESIAN_POINT('Origin',(16.,0.,0.));
#25457=CARTESIAN_POINT('',(16.,-20.,-2.44929359829471E-15));
#25458=CARTESIAN_POINT('Origin',(16.,0.,0.));
#25459=CARTESIAN_POINT('Origin',(29.6565816563128,24.25,24.8693842857571));
#25460=CARTESIAN_POINT('',(24.0627188904386,24.5,41.2765066351308));
#25461=CARTESIAN_POINT('',(29.418817527239,24.5,24.7921300371634));
#25462=CARTESIAN_POINT('Origin',(63.2350933817184,0.,0.));
#25463=CARTESIAN_POINT('Origin',(42.5,0.,0.));
#25464=CARTESIAN_POINT('',(42.5,24.5,41.2765066351308));
#25465=CARTESIAN_POINT('Origin',(42.5,0.,0.));
#25466=CARTESIAN_POINT('',(42.5,-20.,-2.44929359829471E-15));
#25467=CARTESIAN_POINT('Origin',(34.9605325577062,24.5,0.));
#25468=CARTESIAN_POINT('',(0.,0.,0.));
#25469=CARTESIAN_POINT('Origin',(65.9767766952966,0.,-1.28139550481832E-15));
#25470=CARTESIAN_POINT('',(66.1535533905933,41.8535533905933,-5.12558201927329E-15));
#25471=CARTESIAN_POINT('',(66.1535533905933,-41.8535533905933,-5.12558201927329E-15));
#25472=CARTESIAN_POINT('Origin',(66.1535533905933,0.,-2.56279100963665E-15));
#25473=CARTESIAN_POINT('Origin',(66.1535533905933,0.,-2.56279100963665E-15));
#25474=CARTESIAN_POINT('',(65.8,41.,5.02105187650415E-15));
#25475=CARTESIAN_POINT('',(65.9767766952966,41.4267766952966,5.07331694788872E-15));
#25476=CARTESIAN_POINT('Origin',(65.8,0.,0.));
#25477=CARTESIAN_POINT('Origin',(65.8,41.5,0.));
#25478=CARTESIAN_POINT('',(65.8,-1.0421744260744E-15,36.51));
#25479=CARTESIAN_POINT('Origin',(65.8,0.,28.));
#25480=CARTESIAN_POINT('',(65.8,-28.5446674249078,22.7636126658624));
#25481=CARTESIAN_POINT('Origin',(65.8,-21.8912815091048,17.4577144520445));
#25482=CARTESIAN_POINT('',(65.8,-35.5946180737584,-8.12423929874504));
#25483=CARTESIAN_POINT('Origin',(65.8,-27.2979815410911,-6.2305861507768));
#25484=CARTESIAN_POINT('',(65.8,-15.8410953151821,-32.8943733671173));
#25485=CARTESIAN_POINT('Origin',(65.8,-12.1487446952916,-25.2271283012677));
#25486=CARTESIAN_POINT('',(65.8,15.841095315182,-32.8943733671173));
#25487=CARTESIAN_POINT('Origin',(65.8,12.1487446952916,-25.2271283012677));
#25488=CARTESIAN_POINT('',(65.8,35.5946180737584,-8.12423929874504));
#25489=CARTESIAN_POINT('Origin',(65.8,27.2979815410911,-6.23058615077681));
#25490=CARTESIAN_POINT('',(65.8,28.5446674249078,22.7636126658624));
#25491=CARTESIAN_POINT('Origin',(65.8,21.8912815091048,17.4577144520445));
#25492=CARTESIAN_POINT('',(65.8,-3.525,12.0031027238794));
#25493=CARTESIAN_POINT('',(65.8,-3.525,16.1));
#25494=CARTESIAN_POINT('',(65.8,-3.525,6.));
#25495=CARTESIAN_POINT('',(65.8,3.525,12.0031027238794));
#25496=CARTESIAN_POINT('Origin',(65.8,0.,0.));
#25497=CARTESIAN_POINT('',(65.8,3.525,16.1));
#25498=CARTESIAN_POINT('',(65.8,3.525,6.));
#25499=CARTESIAN_POINT('',(65.8,20.75,16.1));
#25500=CARTESIAN_POINT('Origin',(66.3,0.,0.));
#25501=CARTESIAN_POINT('',(66.8,-42.5,-5.20474889637625E-15));
#25502=CARTESIAN_POINT('Origin',(66.8,0.,0.));
#25503=CARTESIAN_POINT('',(66.3,-42.,-5.14351655641888E-15));
#25504=CARTESIAN_POINT('Origin',(66.05,-3.275,6.));
#25505=CARTESIAN_POINT('',(66.3,-3.025,15.6));
#25506=CARTESIAN_POINT('',(66.3,-3.025,12.1387592034771));
#25507=CARTESIAN_POINT('',(66.3,-3.025,6.));
#25508=CARTESIAN_POINT('Origin',(69.3249999999999,0.,0.));
#25509=CARTESIAN_POINT('',(65.8,-3.525,16.1));
#25510=CARTESIAN_POINT('Origin',(66.05,3.275,6.));
#25511=CARTESIAN_POINT('',(66.3,3.025,12.1387592034771));
#25512=CARTESIAN_POINT('Origin',(69.3249999999999,0.,0.));
#25513=CARTESIAN_POINT('',(66.3,3.025,15.6));
#25514=CARTESIAN_POINT('',(66.3,3.025,6.));
#25515=CARTESIAN_POINT('',(66.3,3.025,15.6));
#25516=CARTESIAN_POINT('Origin',(66.05,20.75,15.85));
#25517=CARTESIAN_POINT('',(66.3,20.75,15.6));
#25518=CARTESIAN_POINT('Origin',(65.7,-3.025,12.));
#25519=CARTESIAN_POINT('',(125.3,-3.025,15.6));
#25520=CARTESIAN_POINT('',(65.7,-3.025,15.6));
#25521=CARTESIAN_POINT('',(125.3,-3.025,12.1387592034771));
#25522=CARTESIAN_POINT('',(125.3,-3.025,6.));
#25523=CARTESIAN_POINT('',(95.8,-3.025,12.1387592034771));
#25524=CARTESIAN_POINT('Origin',(95.8,0.,15.6));
#25525=CARTESIAN_POINT('',(125.3,3.025,15.6));
#25526=CARTESIAN_POINT('',(125.9,3.025,15.6));
#25527=CARTESIAN_POINT('',(125.3,6.255,15.6));
#25528=CARTESIAN_POINT('Origin',(95.8,0.,0.));
#25529=CARTESIAN_POINT('',(125.8,-3.525,12.0031027238794));
#25530=CARTESIAN_POINT('Origin',(122.275,0.,0.));
#25531=CARTESIAN_POINT('',(125.8,3.525,12.0031027238794));
#25532=CARTESIAN_POINT('Origin',(125.8,0.,0.));
#25533=CARTESIAN_POINT('',(125.3,3.025,12.1387592034771));
#25534=CARTESIAN_POINT('Origin',(122.275,0.,0.));
#25535=CARTESIAN_POINT('',(95.8,3.025,12.1387592034771));
#25536=CARTESIAN_POINT('Origin',(125.9,3.025,12.));
#25537=CARTESIAN_POINT('',(125.3,3.025,6.));
#25538=CARTESIAN_POINT('Origin',(125.55,-3.275,6.));
#25539=CARTESIAN_POINT('',(125.8,-3.525,16.1));
#25540=CARTESIAN_POINT('',(125.8,-3.525,6.));
#25541=CARTESIAN_POINT('',(125.3,-3.025,15.6));
#25542=CARTESIAN_POINT('Origin',(125.55,3.275,6.));
#25543=CARTESIAN_POINT('',(125.8,3.525,16.1));
#25544=CARTESIAN_POINT('',(125.8,3.525,6.));
#25545=CARTESIAN_POINT('',(125.8,3.525,16.1));
#25546=CARTESIAN_POINT('Origin',(125.55,6.255,15.85));
#25547=CARTESIAN_POINT('',(125.8,6.255,16.1));
#25548=CARTESIAN_POINT('Origin',(125.8,12.51,0.));
#25549=CARTESIAN_POINT('',(125.8,-42.5,-5.20474889637625E-15));
#25550=CARTESIAN_POINT('Origin',(125.8,0.,0.));
#25551=CARTESIAN_POINT('',(125.8,-6.12323399573677E-16,33.));
#25552=CARTESIAN_POINT('Origin',(125.8,0.,28.));
#25553=CARTESIAN_POINT('',(125.8,-25.800438921445,20.5751634613382));
#25554=CARTESIAN_POINT('Origin',(125.8,-21.8912815091048,17.4577144520445));
#25555=CARTESIAN_POINT('',(125.8,-32.1726211020002,-7.34319082055837));
#25556=CARTESIAN_POINT('Origin',(125.8,-27.2979815410911,-6.2305861507768));
#25557=CARTESIAN_POINT('',(125.8,-14.3181633908794,-29.7319726407798));
#25558=CARTESIAN_POINT('Origin',(125.8,-12.1487446952916,-25.2271283012677));
#25559=CARTESIAN_POINT('',(125.8,14.3181633908794,-29.7319726407798));
#25560=CARTESIAN_POINT('Origin',(125.8,12.1487446952916,-25.2271283012677));
#25561=CARTESIAN_POINT('',(125.8,32.1726211020002,-7.34319082055838));
#25562=CARTESIAN_POINT('Origin',(125.8,27.2979815410911,-6.23058615077681));
#25563=CARTESIAN_POINT('',(125.8,25.800438921445,20.5751634613382));
#25564=CARTESIAN_POINT('Origin',(125.8,21.8912815091048,17.4577144520445));
#25565=CARTESIAN_POINT('Origin',(125.8,21.8912815091048,17.4577144520445));
#25566=CARTESIAN_POINT('',(119.,25.800438921445,20.5751634613382));
#25567=CARTESIAN_POINT('',(125.8,25.800438921445,20.5751634613382));
#25568=CARTESIAN_POINT('Origin',(119.,21.8912815091048,17.4577144520445));
#25569=CARTESIAN_POINT('Origin',(65.8,21.8912815091048,17.4577144520445));
#25570=CARTESIAN_POINT('',(119.,28.5446674249078,22.7636126658624));
#25571=CARTESIAN_POINT('',(65.8,28.5446674249078,22.7636126658624));
#25572=CARTESIAN_POINT('Origin',(119.,21.8912815091048,17.4577144520445));
#25573=CARTESIAN_POINT('Origin',(119.,21.8912815091048,17.4577144520445));
#25574=CARTESIAN_POINT('Origin',(125.8,27.2979815410911,-6.23058615077681));
#25575=CARTESIAN_POINT('',(119.,32.1726211020002,-7.34319082055838));
#25576=CARTESIAN_POINT('',(125.8,32.1726211020002,-7.34319082055838));
#25577=CARTESIAN_POINT('Origin',(119.,27.2979815410911,-6.23058615077681));
#25578=CARTESIAN_POINT('Origin',(65.8,27.2979815410911,-6.23058615077681));
#25579=CARTESIAN_POINT('',(119.,35.5946180737584,-8.12423929874504));
#25580=CARTESIAN_POINT('',(65.8,35.5946180737584,-8.12423929874504));
#25581=CARTESIAN_POINT('Origin',(119.,27.2979815410911,-6.23058615077681));
#25582=CARTESIAN_POINT('Origin',(119.,27.2979815410911,-6.23058615077681));
#25583=CARTESIAN_POINT('Origin',(125.8,12.1487446952916,-25.2271283012677));
#25584=CARTESIAN_POINT('',(119.,14.3181633908794,-29.7319726407798));
#25585=CARTESIAN_POINT('',(125.8,14.3181633908794,-29.7319726407798));
#25586=CARTESIAN_POINT('Origin',(119.,12.1487446952916,-25.2271283012677));
#25587=CARTESIAN_POINT('Origin',(65.8,12.1487446952916,-25.2271283012677));
#25588=CARTESIAN_POINT('',(119.,15.841095315182,-32.8943733671173));
#25589=CARTESIAN_POINT('',(65.8,15.841095315182,-32.8943733671173));
#25590=CARTESIAN_POINT('Origin',(119.,12.1487446952916,-25.2271283012677));
#25591=CARTESIAN_POINT('Origin',(119.,12.1487446952916,-25.2271283012677));
#25592=CARTESIAN_POINT('Origin',(125.8,-12.1487446952916,-25.2271283012677));
#25593=CARTESIAN_POINT('',(119.,-14.3181633908794,-29.7319726407798));
#25594=CARTESIAN_POINT('',(125.8,-14.3181633908794,-29.7319726407798));
#25595=CARTESIAN_POINT('Origin',(119.,-12.1487446952916,-25.2271283012677));
#25596=CARTESIAN_POINT('Origin',(65.8,-12.1487446952916,-25.2271283012677));
#25597=CARTESIAN_POINT('',(119.,-15.8410953151821,-32.8943733671173));
#25598=CARTESIAN_POINT('',(65.8,-15.8410953151821,-32.8943733671173));
#25599=CARTESIAN_POINT('Origin',(119.,-12.1487446952916,-25.2271283012677));
#25600=CARTESIAN_POINT('Origin',(119.,-12.1487446952916,-25.2271283012677));
#25601=CARTESIAN_POINT('Origin',(125.8,-27.2979815410911,-6.2305861507768));
#25602=CARTESIAN_POINT('',(119.,-32.1726211020002,-7.34319082055837));
#25603=CARTESIAN_POINT('',(125.8,-32.1726211020002,-7.34319082055837));
#25604=CARTESIAN_POINT('Origin',(119.,-27.2979815410911,-6.2305861507768));
#25605=CARTESIAN_POINT('Origin',(65.8,-27.2979815410911,-6.2305861507768));
#25606=CARTESIAN_POINT('',(119.,-35.5946180737584,-8.12423929874504));
#25607=CARTESIAN_POINT('',(65.8,-35.5946180737584,-8.12423929874504));
#25608=CARTESIAN_POINT('Origin',(119.,-27.2979815410911,-6.2305861507768));
#25609=CARTESIAN_POINT('Origin',(119.,-27.2979815410911,-6.2305861507768));
#25610=CARTESIAN_POINT('Origin',(125.8,-21.8912815091048,17.4577144520445));
#25611=CARTESIAN_POINT('',(119.,-25.800438921445,20.5751634613382));
#25612=CARTESIAN_POINT('',(125.8,-25.800438921445,20.5751634613382));
#25613=CARTESIAN_POINT('Origin',(119.,-21.8912815091048,17.4577144520445));
#25614=CARTESIAN_POINT('Origin',(65.8,-21.8912815091048,17.4577144520445));
#25615=CARTESIAN_POINT('',(119.,-28.5446674249078,22.7636126658624));
#25616=CARTESIAN_POINT('',(65.8,-28.5446674249078,22.7636126658624));
#25617=CARTESIAN_POINT('Origin',(119.,-21.8912815091048,17.4577144520445));
#25618=CARTESIAN_POINT('Origin',(119.,-21.8912815091048,17.4577144520445));
#25619=CARTESIAN_POINT('Origin',(125.8,0.,28.));
#25620=CARTESIAN_POINT('',(119.,-6.12323399573677E-16,33.));
#25621=CARTESIAN_POINT('',(125.8,6.12323399573677E-16,33.));
#25622=CARTESIAN_POINT('Origin',(119.,0.,28.));
#25623=CARTESIAN_POINT('Origin',(65.8,0.,28.));
#25624=CARTESIAN_POINT('',(119.,-1.0421744260744E-15,36.51));
#25625=CARTESIAN_POINT('',(65.8,-1.0421744260744E-15,36.51));
#25626=CARTESIAN_POINT('Origin',(119.,0.,28.));
#25627=CARTESIAN_POINT('Origin',(119.,0.,28.));
#25628=CARTESIAN_POINT('Origin',(96.3,0.,0.));
#25629=CARTESIAN_POINT('',(96.3,-42.5,-5.20474889637625E-15));
#25630=CARTESIAN_POINT('',(0.,0.,0.));
#25631=CARTESIAN_POINT('Origin',(129.7,4.69307322189799,17.9011580382799));
#25632=CARTESIAN_POINT('',(129.8,5.75942780780634,22.2672178622896));
#25633=CARTESIAN_POINT('',(129.6,5.95283803735798,22.2162940046486));
#25634=CARTESIAN_POINT('Origin',(129.6,-2.22044604925031E-15,0.));
#25635=CARTESIAN_POINT('',(129.6,8.54102848838318,31.8755522675393));
#25636=CARTESIAN_POINT('',(129.6,4.78966580452689,17.8752761337696));
#25637=CARTESIAN_POINT('',(129.8,8.3476864616576,31.9267306615923));
#25638=CARTESIAN_POINT('Origin',(129.6,0.,4.44089209850063E-15));
#25639=CARTESIAN_POINT('',(129.8,4.59648063926908,17.9270399427901));
#25640=CARTESIAN_POINT('Origin',(125.8,8.54102848838318,31.8755522675393));
#25641=CARTESIAN_POINT('',(126.,5.95283803735798,22.2162940046486));
#25642=CARTESIAN_POINT('',(125.8,5.95283803735798,22.2162940046486));
#25643=CARTESIAN_POINT('',(126.,8.54102848838318,31.8755522675393));
#25644=CARTESIAN_POINT('',(126.,5.71074115350888,21.3127761337696));
#25645=CARTESIAN_POINT('',(125.8,8.54102848838318,31.8755522675393));
#25646=CARTESIAN_POINT('Origin',(125.9,5.61414857087997,21.3386580382799));
#25647=CARTESIAN_POINT('',(125.8,8.3476864616576,31.9267306615923));
#25648=CARTESIAN_POINT('Origin',(126.,0.,4.44089209850063E-15));
#25649=CARTESIAN_POINT('',(125.8,5.75942780780634,22.2672178622896));
#25650=CARTESIAN_POINT('Origin',(126.,-2.22044604925031E-15,0.));
#25651=CARTESIAN_POINT('',(125.8,5.51755598825106,21.3645399427901));
#25652=CARTESIAN_POINT('Origin',(129.7,3.39897799638539,-13.0715289068345));
#25653=CARTESIAN_POINT('',(129.8,8.34768646165761,-31.9267306615923));
#25654=CARTESIAN_POINT('',(129.6,8.54102848838319,-31.8755522675393));
#25655=CARTESIAN_POINT('Origin',(129.6,0.,4.44089209850063E-15));
#25656=CARTESIAN_POINT('',(129.6,5.95283803735798,-22.2162940046486));
#25657=CARTESIAN_POINT('',(129.6,3.49557057901429,-13.0456470023243));
#25658=CARTESIAN_POINT('',(129.8,5.75942780780635,-22.2672178622896));
#25659=CARTESIAN_POINT('Origin',(129.6,-2.22044604925031E-15,0.));
#25660=CARTESIAN_POINT('',(129.8,3.30238541375648,-13.0974108113448));
#25661=CARTESIAN_POINT('Origin',(125.8,5.95283803735798,-22.2162940046486));
#25662=CARTESIAN_POINT('',(126.,8.54102848838319,-31.8755522675393));
#25663=CARTESIAN_POINT('',(125.8,8.54102848838319,-31.8755522675393));
#25664=CARTESIAN_POINT('',(126.,5.95283803735798,-22.2162940046486));
#25665=CARTESIAN_POINT('',(126.,4.41664592799628,-16.4831470023243));
#25666=CARTESIAN_POINT('',(125.8,5.95283803735798,-22.2162940046486));
#25667=CARTESIAN_POINT('Origin',(125.9,4.32005334536737,-16.5090289068345));
#25668=CARTESIAN_POINT('',(125.8,5.75942780780635,-22.2672178622896));
#25669=CARTESIAN_POINT('Origin',(126.,-2.22044604925031E-15,0.));
#25670=CARTESIAN_POINT('',(125.8,8.34768646165761,-31.9267306615923));
#25671=CARTESIAN_POINT('Origin',(126.,0.,4.44089209850063E-15));
#25672=CARTESIAN_POINT('',(125.8,4.22346076273846,-16.5349108113448));
#25673=CARTESIAN_POINT('Origin',(129.7,-3.65477010122739,-14.0261580382799));
#25674=CARTESIAN_POINT('',(129.8,-5.75942780780635,-22.2672178622896));
#25675=CARTESIAN_POINT('',(129.6,-5.95283803735798,-22.2162940046486));
#25676=CARTESIAN_POINT('Origin',(129.6,0.,0.));
#25677=CARTESIAN_POINT('',(129.6,-8.54102848838319,-31.8755522675393));
#25678=CARTESIAN_POINT('',(129.6,-3.75136268385629,-14.0002761337696));
#25679=CARTESIAN_POINT('',(129.8,-8.34768646165761,-31.9267306615923));
#25680=CARTESIAN_POINT('Origin',(129.6,0.,-6.66133814775094E-15));
#25681=CARTESIAN_POINT('',(129.8,-3.55817751859848,-14.0520399427901));
#25682=CARTESIAN_POINT('Origin',(125.8,-8.54102848838319,-31.8755522675393));
#25683=CARTESIAN_POINT('',(126.,-5.95283803735798,-22.2162940046486));
#25684=CARTESIAN_POINT('',(125.8,-5.95283803735798,-22.2162940046486));
#25685=CARTESIAN_POINT('',(126.,-8.54102848838319,-31.8755522675393));
#25686=CARTESIAN_POINT('',(126.,-2.83028733487431,-10.5627761337696));
#25687=CARTESIAN_POINT('',(125.8,-8.54102848838319,-31.8755522675393));
#25688=CARTESIAN_POINT('Origin',(125.9,-2.7336947522454,-10.5886580382799));
#25689=CARTESIAN_POINT('',(125.8,-8.34768646165762,-31.9267306615923));
#25690=CARTESIAN_POINT('Origin',(126.,0.,-6.66133814775094E-15));
#25691=CARTESIAN_POINT('',(125.8,-5.75942780780634,-22.2672178622896));
#25692=CARTESIAN_POINT('Origin',(126.,0.,0.));
#25693=CARTESIAN_POINT('',(125.8,-2.6371021696165,-10.6145399427901));
#25694=CARTESIAN_POINT('Origin',(129.7,-2.36067487571478,9.19652890683454));
#25695=CARTESIAN_POINT('',(129.8,-8.3476864616576,31.9267306615923));
#25696=CARTESIAN_POINT('',(129.6,-8.54102848838318,31.8755522675393));
#25697=CARTESIAN_POINT('Origin',(129.6,0.,-6.66133814775094E-15));
#25698=CARTESIAN_POINT('',(129.6,-5.95283803735798,22.2162940046486));
#25699=CARTESIAN_POINT('',(129.6,-2.45726745834369,9.17064700232429));
#25700=CARTESIAN_POINT('',(129.8,-5.75942780780634,22.2672178622896));
#25701=CARTESIAN_POINT('Origin',(129.6,0.,0.));
#25702=CARTESIAN_POINT('',(129.8,-2.26408229308588,9.22241081134479));
#25703=CARTESIAN_POINT('Origin',(125.8,-5.95283803735798,22.2162940046486));
#25704=CARTESIAN_POINT('',(126.,-8.54102848838318,31.8755522675393));
#25705=CARTESIAN_POINT('',(125.8,-8.54102848838318,31.8755522675393));
#25706=CARTESIAN_POINT('',(126.,-5.95283803735798,22.2162940046486));
#25707=CARTESIAN_POINT('',(126.,-1.53619210936171,5.73314700232429));
#25708=CARTESIAN_POINT('',(125.8,-5.95283803735798,22.2162940046486));
#25709=CARTESIAN_POINT('Origin',(125.9,-1.4395995267328,5.75902890683454));
#25710=CARTESIAN_POINT('',(125.8,-5.75942780780634,22.2672178622896));
#25711=CARTESIAN_POINT('Origin',(126.,0.,0.));
#25712=CARTESIAN_POINT('',(125.8,-8.34768646165761,31.9267306615923));
#25713=CARTESIAN_POINT('Origin',(126.,0.,-6.66133814775094E-15));
#25714=CARTESIAN_POINT('',(125.8,-1.3430069441039,5.78491081134479));
#25715=CARTESIAN_POINT('Origin',(125.8,0.,-6.66133814775094E-15));
#25716=CARTESIAN_POINT('Origin',(125.8,0.,-6.66133814775094E-15));
#25717=CARTESIAN_POINT('Origin',(129.8,0.,-6.66133814775094E-15));
#25718=CARTESIAN_POINT('Origin',(125.8,0.,0.));
#25719=CARTESIAN_POINT('Origin',(125.8,0.,0.));
#25720=CARTESIAN_POINT('Origin',(129.8,0.,0.));
#25721=CARTESIAN_POINT('Origin',(125.8,0.,4.44089209850063E-15));
#25722=CARTESIAN_POINT('Origin',(125.8,0.,4.44089209850063E-15));
#25723=CARTESIAN_POINT('Origin',(129.8,0.,4.44089209850063E-15));
#25724=CARTESIAN_POINT('Origin',(125.8,-2.22044604925031E-15,0.));
#25725=CARTESIAN_POINT('Origin',(125.8,-2.22044604925031E-15,0.));
#25726=CARTESIAN_POINT('Origin',(129.8,-2.22044604925031E-15,0.));
#25727=CARTESIAN_POINT('Origin',(127.8,0.,0.));
#25728=CARTESIAN_POINT('',(129.8,-15.5,-1.8982025386784E-15));
#25729=CARTESIAN_POINT('Origin',(129.8,0.,0.));
#25730=CARTESIAN_POINT('',(125.8,-15.5,-1.8982025386784E-15));
#25731=CARTESIAN_POINT('',(127.8,-15.5,-1.8982025386784E-15));
#25732=CARTESIAN_POINT('Origin',(125.8,0.,0.));
#25733=CARTESIAN_POINT('Origin',(125.8,43.,0.));
#25734=CARTESIAN_POINT('',(125.8,-43.,-5.26598123633362E-15));
#25735=CARTESIAN_POINT('Origin',(125.8,0.,0.));
#25736=CARTESIAN_POINT('Origin',(127.8,0.,0.));
#25737=CARTESIAN_POINT('',(129.8,-43.,-5.26598123633362E-15));
#25738=CARTESIAN_POINT('Origin',(129.8,0.,0.));
#25739=CARTESIAN_POINT('',(127.8,-43.,-5.26598123633362E-15));
#25740=CARTESIAN_POINT('Origin',(129.8,15.5,0.));
#25741=CARTESIAN_POINT('',(0.,0.,0.));
#25742=CARTESIAN_POINT('Origin',(-24.9,7.95870312499776,7.37391828833597));
#25743=CARTESIAN_POINT('',(-16.2963973586152,7.92227791262654,7.04797145648968));
#25744=CARTESIAN_POINT('',(-41.2927947172303,7.92227791262654,7.04797145648968));
#25745=CARTESIAN_POINT('',(-24.9,7.92227791262654,7.04797145648968));
#25746=CARTESIAN_POINT('',(-40.3,7.99512833736898,7.69986512018227));
#25747=CARTESIAN_POINT('Ctrl Pts',(-41.2927947172303,7.92227791262654,7.04797145648968));
#25748=CARTESIAN_POINT('Ctrl Pts',(-40.8162222946068,7.95787002002863,7.36646334414742));
#25749=CARTESIAN_POINT('Ctrl Pts',(-40.3,7.99512833736897,7.69986512018227));
#25750=CARTESIAN_POINT('',(-15.8,7.99512833736898,7.69986512018227));
#25751=CARTESIAN_POINT('',(-24.9,7.99512833736897,7.69986512018227));
#25752=CARTESIAN_POINT('Ctrl Pts',(-15.8,7.99512833736897,7.69986512018227));
#25753=CARTESIAN_POINT('Ctrl Pts',(-15.9670634484609,7.97101274591251,7.48406951813534));
#25754=CARTESIAN_POINT('Ctrl Pts',(-16.1329130514351,7.94669708059969,7.26648357815028));
#25755=CARTESIAN_POINT('Ctrl Pts',(-16.2963973586152,7.92227791262654,7.04797145648968));
#25756=CARTESIAN_POINT('Origin',(-24.9,9.71692839447408,4.8266892308878));
#25757=CARTESIAN_POINT('',(-15.8,10.0346105348206,4.74516505660943));
#25758=CARTESIAN_POINT('',(-40.3,10.0346105348206,4.74516505660943));
#25759=CARTESIAN_POINT('',(-24.9,10.0346105348206,4.74516505660943));
#25760=CARTESIAN_POINT('',(-41.2927947172303,9.39924625412754,4.90821340516617));
#25761=CARTESIAN_POINT('Ctrl Pts',(-40.3,10.0346105348206,4.74516505660943));
#25762=CARTESIAN_POINT('Ctrl Pts',(-40.816222294603,9.70966247747854,4.82855382385103));
#25763=CARTESIAN_POINT('Ctrl Pts',(-41.2927947172303,9.39924625412754,4.90821340516617));
#25764=CARTESIAN_POINT('',(-16.2963973586152,9.39924625412754,4.90821340516617));
#25765=CARTESIAN_POINT('',(-24.9,9.39924625412754,4.90821340516617));
#25766=CARTESIAN_POINT('Ctrl Pts',(-16.2963973586152,9.39924625412754,4.90821340516617));
#25767=CARTESIAN_POINT('Ctrl Pts',(-16.1329130514352,9.61221779340456,4.85356025763508));
#25768=CARTESIAN_POINT('Ctrl Pts',(-15.9670634484611,9.82428663522205,4.79913876198385));
#25769=CARTESIAN_POINT('Ctrl Pts',(-15.8,10.0346105348206,4.74516505660943));
#25770=CARTESIAN_POINT('Origin',(-16.05,0.,0.));
#25771=CARTESIAN_POINT('Origin',(-15.8,0.,0.));
#25772=CARTESIAN_POINT('',(-16.3,9.39625879385653,4.90615131023023));
#25773=CARTESIAN_POINT('Ctrl Pts',(-16.2963973586152,9.3992462541275,4.90821340516614));
#25774=CARTESIAN_POINT('Ctrl Pts',(-16.2981989900367,9.39775227019672,4.90718218251594));
#25775=CARTESIAN_POINT('Ctrl Pts',(-16.3,9.39625879385648,4.90615131023019));
#25776=CARTESIAN_POINT('',(-16.3,7.91929045235553,7.04590936155374));
#25777=CARTESIAN_POINT('Origin',(-16.3,0.,0.));
#25778=CARTESIAN_POINT('Ctrl Pts',(-16.3,7.91929045235555,7.04590936155372));
#25779=CARTESIAN_POINT('Ctrl Pts',(-16.2981989900367,7.92078392869578,7.04694023383947));
#25780=CARTESIAN_POINT('Ctrl Pts',(-16.2963973586152,7.92227791262655,7.04797145648966));
#25781=CARTESIAN_POINT('Origin',(-41.3,8.56123351384782,7.48901066372381));
#25782=CARTESIAN_POINT('',(-16.3,7.1621609418286,6.52330059428085));
#25783=CARTESIAN_POINT('',(-16.3,8.56123351384782,7.48901066372381));
#25784=CARTESIAN_POINT('',(-40.8,7.1621609418286,6.52330059428085));
#25785=CARTESIAN_POINT('',(-41.3,7.1621609418286,6.52330059428085));
#25786=CARTESIAN_POINT('',(-41.3,6.75066900888177,6.23926822091527));
#25787=CARTESIAN_POINT('',(-40.625,7.30618311835999,6.6227119249588));
#25788=CARTESIAN_POINT('',(-41.3,7.91929045235552,7.04590936155373));
#25789=CARTESIAN_POINT('',(-41.3,7.50107762221138,6.75723788780913));
#25790=CARTESIAN_POINT('Ctrl Pts',(-41.2927947172303,7.92227791262654,7.04797145648968));
#25791=CARTESIAN_POINT('Ctrl Pts',(-41.2963979800735,7.92078392869575,7.04694023383948));
#25792=CARTESIAN_POINT('Ctrl Pts',(-41.3,7.91929045235552,7.04590936155373));
#25793=CARTESIAN_POINT('Origin',(-16.3,8.60018139858871,5.93627660334058));
#25794=CARTESIAN_POINT('',(-16.3,8.63912928332961,4.38354254295734));
#25795=CARTESIAN_POINT('',(-16.3,8.63912928332961,4.38354254295734));
#25796=CARTESIAN_POINT('',(-16.3,7.1621609418286,6.52330059428085));
#25797=CARTESIAN_POINT('Origin',(-41.3,8.63912928332961,4.38354254295734));
#25798=CARTESIAN_POINT('',(-41.3,9.39625879385652,4.90615131023022));
#25799=CARTESIAN_POINT('Ctrl Pts',(-41.3,9.39625879385652,4.90615131023023));
#25800=CARTESIAN_POINT('Ctrl Pts',(-41.2963979800735,9.39775227019676,4.90718218251597));
#25801=CARTESIAN_POINT('Ctrl Pts',(-41.2927947172303,9.39924625412754,4.90821340516617));
#25802=CARTESIAN_POINT('',(-41.3,8.22763735038278,4.09951016959176));
#25803=CARTESIAN_POINT('',(-41.3,8.27850967770278,4.13462480176414));
#25804=CARTESIAN_POINT('',(-40.8,8.63912928332961,4.38354254295734));
#25805=CARTESIAN_POINT('',(-41.05,8.43338331685619,4.24152635627455));
#25806=CARTESIAN_POINT('',(-41.3,8.63912928332961,4.38354254295734));
#25807=CARTESIAN_POINT('Origin',(-24.9,10.4739123357613,2.83068661947788));
#25808=CARTESIAN_POINT('',(-16.2963973586152,10.2901843663683,2.55900267341252));
#25809=CARTESIAN_POINT('',(-41.2927947172303,10.2901843663683,2.55900267341252));
#25810=CARTESIAN_POINT('',(-24.9,10.2901843663683,2.55900267341252));
#25811=CARTESIAN_POINT('',(-40.3,10.6576403051544,3.10237056554323));
#25812=CARTESIAN_POINT('Ctrl Pts',(-41.2927947172303,10.2901843663683,2.55900267341252));
#25813=CARTESIAN_POINT('Ctrl Pts',(-40.8162222946067,10.4697101726358,2.82447275740919));
#25814=CARTESIAN_POINT('Ctrl Pts',(-40.3,10.6576403051544,3.10237056554323));
#25815=CARTESIAN_POINT('',(-15.8,10.6576403051544,3.10237056554323));
#25816=CARTESIAN_POINT('',(-24.9,10.6576403051544,3.10237056554323));
#25817=CARTESIAN_POINT('Ctrl Pts',(-15.8,10.6576403051544,3.10237056554324));
#25818=CARTESIAN_POINT('Ctrl Pts',(-15.9670634484609,10.5360017926907,2.92250012355864));
#25819=CARTESIAN_POINT('Ctrl Pts',(-16.1329130514351,10.4133541120997,2.741137395016));
#25820=CARTESIAN_POINT('Ctrl Pts',(-16.2963973586152,10.2901843663683,2.55900267341252));
#25821=CARTESIAN_POINT('Origin',(-24.9,10.8469871275755,-0.241860722557101));
#25822=CARTESIAN_POINT('',(-15.8,11.0903945201189,-0.461681045871784));
#25823=CARTESIAN_POINT('',(-40.3,11.0903945201189,-0.461681045871784));
#25824=CARTESIAN_POINT('',(-24.9,11.0903945201189,-0.461681045871784));
#25825=CARTESIAN_POINT('',(-41.2927947172303,10.6035797350322,-0.0220403992424186));
#25826=CARTESIAN_POINT('Ctrl Pts',(-40.3,11.0903945201189,-0.461681045871779));
#25827=CARTESIAN_POINT('Ctrl Pts',(-40.816222294603,10.8414199971464,-0.236833067488454));
#25828=CARTESIAN_POINT('Ctrl Pts',(-41.2927947172303,10.6035797350322,-0.0220403992424186));
#25829=CARTESIAN_POINT('',(-16.2963973586152,10.6035797350322,-0.0220403992424183));
#25830=CARTESIAN_POINT('',(-24.9,10.6035797350322,-0.0220403992424183));
#25831=CARTESIAN_POINT('Ctrl Pts',(-16.2963973586152,10.6035797350322,-0.022040399242419));
#25832=CARTESIAN_POINT('Ctrl Pts',(-16.1329130514351,10.7667580836949,-0.169406167332656));
#25833=CARTESIAN_POINT('Ctrl Pts',(-15.9670634484609,10.9292447874492,-0.316147313443247));
#25834=CARTESIAN_POINT('Ctrl Pts',(-15.8,11.0903945201189,-0.461681045871786));
#25835=CARTESIAN_POINT('Origin',(-16.05,0.,0.));
#25836=CARTESIAN_POINT('Origin',(-15.8,0.,0.));
#25837=CARTESIAN_POINT('',(-16.3,10.5999761670341,-0.022477951615418));
#25838=CARTESIAN_POINT('Ctrl Pts',(-16.2963973586153,10.6035797350322,-0.0220403992424162));
#25839=CARTESIAN_POINT('Ctrl Pts',(-16.2981989900368,10.6017776448974,-0.0222592126005309));
#25840=CARTESIAN_POINT('Ctrl Pts',(-16.3000000000001,10.5999761670342,-0.0224779516154164));
#25841=CARTESIAN_POINT('',(-16.3,10.2865807983703,2.55856512103952));
#25842=CARTESIAN_POINT('Origin',(-16.3,0.,0.));
#25843=CARTESIAN_POINT('Ctrl Pts',(-16.3000000000001,10.2865807983704,2.55856512103953));
#25844=CARTESIAN_POINT('Ctrl Pts',(-16.2981989900368,10.2883822762336,2.55878386005442));
#25845=CARTESIAN_POINT('Ctrl Pts',(-16.2963973586153,10.2901843663684,2.55900267341253));
#25846=CARTESIAN_POINT('Origin',(-41.3,11.0609125929761,2.65258602321261));
#25847=CARTESIAN_POINT('',(-16.3,9.3733075070094,2.44767366677856));
#25848=CARTESIAN_POINT('',(-16.3,11.0609125929761,2.65258602321261));
#25849=CARTESIAN_POINT('',(-40.8,9.3733075070094,2.44767366677856));
#25850=CARTESIAN_POINT('',(-41.3,9.3733075070094,2.44767366677856));
#25851=CARTESIAN_POINT('',(-41.3,8.87695306996037,2.3874053266509));
#25852=CARTESIAN_POINT('',(-40.625,9.54703155997656,2.46876758582325));
#25853=CARTESIAN_POINT('',(-41.3,10.2865807983703,2.55856512103952));
#25854=CARTESIAN_POINT('',(-41.3,10.6751032705011,2.60574029013207));
#25855=CARTESIAN_POINT('Ctrl Pts',(-41.2927947172303,10.2901843663683,2.55900267341252));
#25856=CARTESIAN_POINT('Ctrl Pts',(-41.2963979800735,10.2883822762335,2.5587838600544));
#25857=CARTESIAN_POINT('Ctrl Pts',(-41.3,10.2865807983703,2.55856512103952));
#25858=CARTESIAN_POINT('Origin',(-16.3,10.3738077343247,1.25960830866812));
#25859=CARTESIAN_POINT('',(-16.3,9.68670287567324,-0.133369405876376));
#25860=CARTESIAN_POINT('',(-16.3,9.68670287567324,-0.133369405876376));
#25861=CARTESIAN_POINT('',(-16.3,9.3733075070094,2.44767366677856));
#25862=CARTESIAN_POINT('Origin',(-41.3,9.68670287567324,-0.133369405876376));
#25863=CARTESIAN_POINT('',(-41.3,10.5999761670341,-0.0224779516154188));
#25864=CARTESIAN_POINT('Ctrl Pts',(-41.3,10.5999761670341,-0.0224779516154188));
#25865=CARTESIAN_POINT('Ctrl Pts',(-41.2963979800734,10.6017776448974,-0.022259212600532));
#25866=CARTESIAN_POINT('Ctrl Pts',(-41.2927947172303,10.6035797350322,-0.0220403992424185));
#25867=CARTESIAN_POINT('',(-41.3,9.19034843862421,-0.193637746004037));
#25868=CARTESIAN_POINT('',(-41.3,10.1446960961816,-0.0777589607398988));
#25869=CARTESIAN_POINT('',(-40.8,9.68670287567324,-0.133369405876376));
#25870=CARTESIAN_POINT('',(-41.05,9.43852565714873,-0.163503575940206));
#25871=CARTESIAN_POINT('',(-41.3,9.68670287567324,-0.133369405876376));
#25872=CARTESIAN_POINT('Origin',(-24.9,10.589674454729,-2.36102124043076));
#25873=CARTESIAN_POINT('',(-16.2963973586152,10.30073359194,-2.51620278281809));
#25874=CARTESIAN_POINT('',(-41.2927947172303,10.30073359194,-2.51620278281809));
#25875=CARTESIAN_POINT('',(-24.9,10.30073359194,-2.51620278281809));
#25876=CARTESIAN_POINT('',(-40.3,10.8786153175179,-2.20583969804344));
#25877=CARTESIAN_POINT('Ctrl Pts',(-41.2927947172303,10.30073359194,-2.51620278281809));
#25878=CARTESIAN_POINT('Ctrl Pts',(-40.8162222946069,10.5830658983774,-2.36457049946494));
#25879=CARTESIAN_POINT('Ctrl Pts',(-40.3,10.8786153175179,-2.20583969804344));
#25880=CARTESIAN_POINT('',(-15.8,10.8786153175179,-2.20583969804344));
#25881=CARTESIAN_POINT('',(-24.9,10.8786153175179,-2.20583969804344));
#25882=CARTESIAN_POINT('Ctrl Pts',(-15.8,10.8786153175179,-2.20583969804343));
#25883=CARTESIAN_POINT('Ctrl Pts',(-15.967063448461,10.6873198013494,-2.30857882938082));
#25884=CARTESIAN_POINT('Ctrl Pts',(-16.1329130514351,10.4944372110389,-2.41217033102974));
#25885=CARTESIAN_POINT('Ctrl Pts',(-16.2963973586152,10.30073359194,-2.51620278281809));
#25886=CARTESIAN_POINT('Origin',(-24.9,9.49213183011501,-5.25500329920184));
#25887=CARTESIAN_POINT('',(-15.8,9.60550277460058,-5.56276158460351));
#25888=CARTESIAN_POINT('',(-40.3,9.60550277460058,-5.56276158460351));
#25889=CARTESIAN_POINT('',(-24.9,9.60550277460058,-5.56276158460351));
#25890=CARTESIAN_POINT('',(-41.2927947172303,9.37876088562945,-4.94724501380017));
#25891=CARTESIAN_POINT('Ctrl Pts',(-40.3,9.60550277460057,-5.56276158460351));
#25892=CARTESIAN_POINT('Ctrl Pts',(-40.8162222946031,9.48953884874235,-5.24796435721412));
#25893=CARTESIAN_POINT('Ctrl Pts',(-41.2927947172303,9.37876088562945,-4.94724501380017));
#25894=CARTESIAN_POINT('',(-16.2963973586152,9.37876088562945,-4.94724501380017));
#25895=CARTESIAN_POINT('',(-24.9,9.37876088562945,-4.94724501380017));
#25896=CARTESIAN_POINT('Ctrl Pts',(-16.2963973586152,9.37876088562945,-4.94724501380017));
#25897=CARTESIAN_POINT('Ctrl Pts',(-16.1329130514351,9.45476385051142,-5.15356368093007));
#25898=CARTESIAN_POINT('Ctrl Pts',(-15.9670634484609,9.53044467054932,-5.35900784934856));
#25899=CARTESIAN_POINT('Ctrl Pts',(-15.8,9.60550277460058,-5.56276158460352));
#25900=CARTESIAN_POINT('Origin',(-16.05,0.,0.));
#25901=CARTESIAN_POINT('Origin',(-15.8,0.,0.));
#25902=CARTESIAN_POINT('',(-16.3,9.37536674390501,-4.94595778563465));
#25903=CARTESIAN_POINT('Ctrl Pts',(-16.2963973586152,9.37876088562946,-4.94724501380016));
#25904=CARTESIAN_POINT('Ctrl Pts',(-16.2981989900368,9.37706352642295,-4.94660129036284));
#25905=CARTESIAN_POINT('Ctrl Pts',(-16.3000000000001,9.37536674390502,-4.94595778563464));
#25906=CARTESIAN_POINT('',(-16.3,10.2973394502156,-2.51491555465257));
#25907=CARTESIAN_POINT('Origin',(-16.3,0.,0.));
#25908=CARTESIAN_POINT('Ctrl Pts',(-16.3,10.2973394502156,-2.51491555465259));
#25909=CARTESIAN_POINT('Ctrl Pts',(-16.2981989900368,10.2990362327336,-2.51555905938079));
#25910=CARTESIAN_POINT('Ctrl Pts',(-16.2963973586152,10.3007335919401,-2.51620278281811));
#25911=CARTESIAN_POINT('Origin',(-41.3,11.0266698955005,-2.79151410808962));
#25912=CARTESIAN_POINT('',(-16.3,9.43714228293528,-2.18868580011731));
#25913=CARTESIAN_POINT('',(-16.3,11.0266698955005,-2.79151410808962));
#25914=CARTESIAN_POINT('',(-40.8,9.43714228293528,-2.18868580011731));
#25915=CARTESIAN_POINT('',(-41.3,9.43714228293528,-2.18868580011731));
#25916=CARTESIAN_POINT('',(-41.3,8.96963416159257,-2.01138335659604));
#25917=CARTESIAN_POINT('',(-40.625,9.60077012540523,-2.25074165534975));
#25918=CARTESIAN_POINT('',(-41.3,10.2973394502156,-2.51491555465257));
#25919=CARTESIAN_POINT('',(-41.3,10.3773816069813,-2.5452715406374));
#25920=CARTESIAN_POINT('Ctrl Pts',(-41.2927947172303,10.30073359194,-2.51620278281809));
#25921=CARTESIAN_POINT('Ctrl Pts',(-41.2963979800735,10.2990362327335,-2.51555905938076));
#25922=CARTESIAN_POINT('Ctrl Pts',(-41.3,10.2973394502156,-2.51491555465257));
#25923=CARTESIAN_POINT('Origin',(-16.3,9.77091973606258,-3.7056210695945));
#25924=CARTESIAN_POINT('',(-16.3,8.51516957662468,-4.61972803109938));
#25925=CARTESIAN_POINT('',(-16.3,8.51516957662468,-4.61972803109938));
#25926=CARTESIAN_POINT('',(-16.3,9.43714228293528,-2.18868580011731));
#25927=CARTESIAN_POINT('Origin',(-41.3,8.51516957662468,-4.61972803109938));
#25928=CARTESIAN_POINT('',(-41.3,9.375366743905,-4.94595778563465));
#25929=CARTESIAN_POINT('Ctrl Pts',(-41.3,9.375366743905,-4.94595778563465));
#25930=CARTESIAN_POINT('Ctrl Pts',(-41.2963979800735,9.37706352642292,-4.94660129036284));
#25931=CARTESIAN_POINT('Ctrl Pts',(-41.2927947172303,9.37876088562945,-4.94724501380017));
#25932=CARTESIAN_POINT('',(-41.3,8.04766145528198,-4.44242558757812));
#25933=CARTESIAN_POINT('',(-41.3,8.66064509438811,-4.67489961763332));
#25934=CARTESIAN_POINT('',(-40.8,8.51516957662468,-4.61972803109938));
#25935=CARTESIAN_POINT('',(-41.05,8.28141551595333,-4.53107680933875));
#25936=CARTESIAN_POINT('',(-41.3,8.51516957662468,-4.61972803109938));
#25937=CARTESIAN_POINT('Origin',(-24.9,8.27946977552995,-7.01184758754715));
#25938=CARTESIAN_POINT('',(-16.2963973586152,7.95150888889516,-7.01497650503583));
#25939=CARTESIAN_POINT('',(-41.2927947172303,7.95150888889516,-7.01497650503583));
#25940=CARTESIAN_POINT('',(-24.9,7.95150888889516,-7.01497650503583));
#25941=CARTESIAN_POINT('',(-40.3,8.60743066216474,-7.00871867005848));
#25942=CARTESIAN_POINT('Ctrl Pts',(-41.2927947172303,7.95150888889516,-7.01497650503583));
#25943=CARTESIAN_POINT('Ctrl Pts',(-40.816222294607,8.2719687665707,-7.01191915107522));
#25944=CARTESIAN_POINT('Ctrl Pts',(-40.3,8.60743066216473,-7.00871867005847));
#25945=CARTESIAN_POINT('',(-15.8,8.60743066216474,-7.00871867005848));
#25946=CARTESIAN_POINT('',(-24.9,8.60743066216474,-7.00871867005848));
#25947=CARTESIAN_POINT('Ctrl Pts',(-15.8,8.60743066216474,-7.00871867005848));
#25948=CARTESIAN_POINT('Ctrl Pts',(-15.967063448461,8.39030163968471,-7.01079019389995));
#25949=CARTESIAN_POINT('Ctrl Pts',(-16.1329130514352,8.17137121660765,-7.01287890404036));
#25950=CARTESIAN_POINT('Ctrl Pts',(-16.2963973586152,7.95150888889516,-7.01497650503583));
#25951=CARTESIAN_POINT('Origin',(-24.9,5.96274352296442,-9.06428794965444));
#25952=CARTESIAN_POINT('',(-15.8,5.92010610227854,-9.38948048284698));
#25953=CARTESIAN_POINT('',(-40.3,5.92010610227854,-9.38948048284698));
#25954=CARTESIAN_POINT('',(-24.9,5.92010610227854,-9.38948048284698));
#25955=CARTESIAN_POINT('',(-41.2927947172303,6.0053809436503,-8.7390954164619));
#25956=CARTESIAN_POINT('Ctrl Pts',(-40.3,5.92010610227854,-9.38948048284697));
#25957=CARTESIAN_POINT('Ctrl Pts',(-40.8162222946032,5.96371871143196,-9.05685025752861));
#25958=CARTESIAN_POINT('Ctrl Pts',(-41.2927947172303,6.0053809436503,-8.7390954164619));
#25959=CARTESIAN_POINT('',(-16.2963973586152,6.0053809436503,-8.7390954164619));
#25960=CARTESIAN_POINT('',(-24.9,6.0053809436503,-8.7390954164619));
#25961=CARTESIAN_POINT('Ctrl Pts',(-16.2963973586152,6.0053809436503,-8.73909541646189));
#25962=CARTESIAN_POINT('Ctrl Pts',(-16.1329130514351,5.97679716143209,-8.95710186240153));
#25963=CARTESIAN_POINT('Ctrl Pts',(-15.9670634484609,5.94833453393568,-9.17418427001393));
#25964=CARTESIAN_POINT('Ctrl Pts',(-15.8,5.92010610227854,-9.38948048284698));
#25965=CARTESIAN_POINT('Origin',(-16.05,0.,0.));
#25966=CARTESIAN_POINT('Origin',(-15.8,0.,0.));
#25967=CARTESIAN_POINT('',(-16.3,6.0029737851647,-8.7363782962178));
#25968=CARTESIAN_POINT('Ctrl Pts',(-16.2963973586153,6.00538094365033,-8.73909541646192));
#25969=CARTESIAN_POINT('Ctrl Pts',(-16.2981989900368,6.00417715991094,-8.73773662551094));
#25970=CARTESIAN_POINT('Ctrl Pts',(-16.3000000000001,6.00297378516472,-8.73637829621782));
#25971=CARTESIAN_POINT('',(-16.3,7.94910173040956,-7.01225938479173));
#25972=CARTESIAN_POINT('Origin',(-16.3,0.,0.));
#25973=CARTESIAN_POINT('Ctrl Pts',(-16.3000000000001,7.94910173040962,-7.01225938479175));
#25974=CARTESIAN_POINT('Ctrl Pts',(-16.2981989900368,7.95030510515584,-7.01361771408487));
#25975=CARTESIAN_POINT('Ctrl Pts',(-16.2963973586152,7.95150888889523,-7.01497650503585));
#25976=CARTESIAN_POINT('Origin',(-41.3,8.46635001074342,-7.59611199862041));
#25977=CARTESIAN_POINT('',(-16.3,7.33904149173406,-6.32364372672954));
#25978=CARTESIAN_POINT('',(-16.3,8.46635001074342,-7.59611199862041));
#25979=CARTESIAN_POINT('',(-40.8,7.33904149173406,-6.32364372672954));
#25980=CARTESIAN_POINT('',(-41.3,7.33904149173406,-6.32364372672954));
#25981=CARTESIAN_POINT('',(-41.3,7.00748016261367,-5.94938835264399));
#25982=CARTESIAN_POINT('',(-40.625,7.4550879569262,-6.45463310765948));
#25983=CARTESIAN_POINT('',(-41.3,7.94910173040956,-7.01225938479173));
#25984=CARTESIAN_POINT('',(-41.3,7.05028478900632,-5.99770478781353));
#25985=CARTESIAN_POINT('Ctrl Pts',(-41.2927947172303,7.95150888889516,-7.01497650503583));
#25986=CARTESIAN_POINT('Ctrl Pts',(-41.2963979800735,7.95030510515576,-7.01361771408484));
#25987=CARTESIAN_POINT('Ctrl Pts',(-41.3,7.94910173040956,-7.01225938479173));
#25988=CARTESIAN_POINT('Origin',(-16.3,6.92963177861631,-7.82193731838801));
#25989=CARTESIAN_POINT('',(-16.3,5.3929135464892,-8.04776263815561));
#25990=CARTESIAN_POINT('',(-16.3,5.3929135464892,-8.04776263815561));
#25991=CARTESIAN_POINT('',(-16.3,7.33904149173406,-6.32364372672954));
#25992=CARTESIAN_POINT('Origin',(-41.3,5.3929135464892,-8.04776263815561));
#25993=CARTESIAN_POINT('',(-41.3,6.00297378516469,-8.7363782962178));
#25994=CARTESIAN_POINT('Ctrl Pts',(-41.3,6.00297378516469,-8.7363782962178));
#25995=CARTESIAN_POINT('Ctrl Pts',(-41.2963979800734,6.00417715991092,-8.73773662551093));
#25996=CARTESIAN_POINT('Ctrl Pts',(-41.2927947172303,6.0053809436503,-8.7390954164619));
#25997=CARTESIAN_POINT('',(-41.3,5.0613522173688,-7.67350726407006));
#25998=CARTESIAN_POINT('',(-41.3,4.54050258425678,-7.08558956329416));
#25999=CARTESIAN_POINT('',(-40.8,5.3929135464892,-8.04776263815561));
#26000=CARTESIAN_POINT('',(-41.05,5.227132881929,-7.86063495111283));
#26001=CARTESIAN_POINT('',(-41.3,5.3929135464892,-8.04776263815561));
#26002=CARTESIAN_POINT('Origin',(-24.9,4.07253834918427,-10.0563441542803));
#26003=CARTESIAN_POINT('',(-41.2927947172303,3.78068932547452,-9.90670364958125));
#26004=CARTESIAN_POINT('',(-40.3,4.36438737289401,-10.2059846589794));
#26005=CARTESIAN_POINT('Ctrl Pts',(-41.2927947172303,3.78068932547452,-9.90670364958125));
#26006=CARTESIAN_POINT('Ctrl Pts',(-40.8162222946071,4.06586327837296,-10.0529216279604));
#26007=CARTESIAN_POINT('Ctrl Pts',(-40.3,4.364387372894,-10.2059846589794));
#26008=CARTESIAN_POINT('',(-15.8,4.36438737289401,-10.2059846589794));
#26009=CARTESIAN_POINT('',(-24.9,4.36438737289401,-10.2059846589794));
#26010=CARTESIAN_POINT('',(-16.2963973586152,3.78068932547452,-9.90670364958125));
#26011=CARTESIAN_POINT('Ctrl Pts',(-16.2963973586435,3.78068932544062,-9.90670364956387));
#26012=CARTESIAN_POINT('Ctrl Pts',(-16.0581111473186,4.06586327835559,-10.0529216279515));
#26013=CARTESIAN_POINT('Ctrl Pts',(-15.8,4.36438737289401,-10.2059846589794));
#26014=CARTESIAN_POINT('',(-24.9,3.78068932547452,-9.90670364958125));
#26015=CARTESIAN_POINT('Origin',(-41.3,3.96649136910327,-10.6605321733406));
#26016=CARTESIAN_POINT('',(-16.3,3.7798206012274,-9.90317909676165));
#26017=CARTESIAN_POINT('Ctrl Pts',(-16.2963973586156,3.78068932547441,-9.90670364958079));
#26018=CARTESIAN_POINT('Ctrl Pts',(-16.2981989900369,3.78025488954973,-9.90494107374806));
#26019=CARTESIAN_POINT('Ctrl Pts',(-16.3,3.7798206012274,-9.90317909676165));
#26020=CARTESIAN_POINT('',(-16.3,3.55965473981442,-9.00993108371628));
#26021=CARTESIAN_POINT('',(-16.3,3.96649136910327,-10.6605321733406));
#26022=CARTESIAN_POINT('',(-40.8,3.55965473981442,-9.00993108371628));
#26023=CARTESIAN_POINT('',(-41.3,3.55965473981442,-9.00993108371628));
#26024=CARTESIAN_POINT('',(-41.3,3.43999690767064,-8.52446017500325));
#26025=CARTESIAN_POINT('',(-40.625,3.60153498106474,-9.17984590176584));
#26026=CARTESIAN_POINT('',(-41.3,3.7798206012274,-9.90317909676164));
#26027=CARTESIAN_POINT('',(-41.3,2.91789939789756,-6.40622731079936));
#26028=CARTESIAN_POINT('Ctrl Pts',(-41.2927947172303,3.78068932547452,-9.90670364958125));
#26029=CARTESIAN_POINT('Ctrl Pts',(-41.2963979800735,3.78025488954977,-9.90494107374824));
#26030=CARTESIAN_POINT('Ctrl Pts',(-41.3,3.7798206012274,-9.90317909676164));
#26031=CARTESIAN_POINT('Origin',(-24.9,1.06736253355198,-10.7970534673528));
#26032=CARTESIAN_POINT('',(-15.8,0.878484466937167,-11.0651825579766));
#26033=CARTESIAN_POINT('',(-40.3,0.878484466937167,-11.0651825579766));
#26034=CARTESIAN_POINT('',(-24.9,0.878484466937167,-11.0651825579766));
#26035=CARTESIAN_POINT('',(-41.2927947172303,1.25624060016678,-10.5289243767289));
#26036=CARTESIAN_POINT('Ctrl Pts',(-40.3,0.878484466937173,-11.0651825579766));
#26037=CARTESIAN_POINT('Ctrl Pts',(-40.816222294603,1.07168248793402,-10.7909209107211));
#26038=CARTESIAN_POINT('Ctrl Pts',(-41.2927947172303,1.25624060016679,-10.5289243767289));
#26039=CARTESIAN_POINT('',(-16.2963973586152,1.25624060016678,-10.5289243767289));
#26040=CARTESIAN_POINT('',(-24.9,1.25624060016678,-10.5289243767289));
#26041=CARTESIAN_POINT('Ctrl Pts',(-16.2963973586152,1.25624060016679,-10.5289243767289));
#26042=CARTESIAN_POINT('Ctrl Pts',(-16.1329130514352,1.12961827088273,-10.7086759519758));
#26043=CARTESIAN_POINT('Ctrl Pts',(-15.9670634484611,1.00353264079967,-10.8876656353246));
#26044=CARTESIAN_POINT('Ctrl Pts',(-15.8,0.878484466937165,-11.0651825579766));
#26045=CARTESIAN_POINT('Origin',(-16.05,0.,0.));
#26046=CARTESIAN_POINT('',(-16.3,1.25537187591967,-10.5253998239093));
#26047=CARTESIAN_POINT('Origin',(-16.3,0.,0.));
#26048=CARTESIAN_POINT('Origin',(-15.8,0.,0.));
#26049=CARTESIAN_POINT('Ctrl Pts',(-16.2963973586152,1.25624060016679,-10.5289243767289));
#26050=CARTESIAN_POINT('Ctrl Pts',(-16.2981989900367,1.25580616424205,-10.5271618008959));
#26051=CARTESIAN_POINT('Ctrl Pts',(-16.3,1.25537187591967,-10.5253998239093));
#26052=CARTESIAN_POINT('Origin',(-41.3,1.03520601450668,-9.63215181086392));
#26053=CARTESIAN_POINT('',(-41.3,1.25537187591967,-10.5253998239093));
#26054=CARTESIAN_POINT('Ctrl Pts',(-41.3,1.25537187591967,-10.5253998239093));
#26055=CARTESIAN_POINT('Ctrl Pts',(-41.2963979800735,1.25580616424204,-10.5271618008959));
#26056=CARTESIAN_POINT('Ctrl Pts',(-41.2927947172303,1.25624060016679,-10.5289243767289));
#26057=CARTESIAN_POINT('',(-41.3,0.915548182362905,-9.1466809021509));
#26058=CARTESIAN_POINT('',(-41.3,0.1900323579454,-6.20314749313486));
#26059=CARTESIAN_POINT('',(-40.8,1.03520601450668,-9.63215181086392));
#26060=CARTESIAN_POINT('',(-41.05,0.975377098434795,-9.38941635650741));
#26061=CARTESIAN_POINT('',(-16.3,1.03520601450668,-9.63215181086392));
#26062=CARTESIAN_POINT('',(-41.3,1.03520601450668,-9.63215181086392));
#26063=CARTESIAN_POINT('',(-16.3,1.03520601450668,-9.63215181086392));
#26064=CARTESIAN_POINT('Origin',(-40.8,0.,0.));
#26065=CARTESIAN_POINT('',(-40.3,-0.878484466937175,-11.0651825579766));
#26066=CARTESIAN_POINT('Origin',(-40.3,0.,0.));
#26067=CARTESIAN_POINT('',(-41.2927947172303,-1.25624060016679,-10.5289243767289));
#26068=CARTESIAN_POINT('Ctrl Pts',(-41.2927947172303,-1.25624060016679,
-10.5289243767289));
#26069=CARTESIAN_POINT('Ctrl Pts',(-40.8162222946063,-1.07168248793539,
-10.7909209107192));
#26070=CARTESIAN_POINT('Ctrl Pts',(-40.3,-0.878484466937179,-11.0651825579766));
#26071=CARTESIAN_POINT('',(-41.3,-1.25537187591967,-10.5253998239093));
#26072=CARTESIAN_POINT('Ctrl Pts',(-41.2927947172303,-1.25624060016679,
-10.5289243767289));
#26073=CARTESIAN_POINT('Ctrl Pts',(-41.2963979800735,-1.25580616424205,
-10.5271618008959));
#26074=CARTESIAN_POINT('Ctrl Pts',(-41.3,-1.25537187591967,-10.5253998239093));
#26075=CARTESIAN_POINT('Origin',(-41.3,0.,0.));
#26076=CARTESIAN_POINT('Origin',(-24.9,0.,0.));
#26077=CARTESIAN_POINT('',(-9.49999999999999,-11.1,-1.35935794705356E-15));
#26078=CARTESIAN_POINT('Origin',(-9.49999999999999,0.,0.));
#26079=CARTESIAN_POINT('',(-15.8,-11.1,-1.35935794705356E-15));
#26080=CARTESIAN_POINT('',(-24.9,-11.1,-1.35935794705356E-15));
#26081=CARTESIAN_POINT('',(-15.8,-11.0903945201189,-0.461681045871775));
#26082=CARTESIAN_POINT('Origin',(-15.8,0.,0.));
#26083=CARTESIAN_POINT('',(-40.3,-11.0903945201189,-0.461681045871775));
#26084=CARTESIAN_POINT('',(-24.9,-11.0903945201189,-0.461681045871775));
#26085=CARTESIAN_POINT('',(-40.3,-10.8786153175179,-2.20583969804343));
#26086=CARTESIAN_POINT('Origin',(-40.3,0.,0.));
#26087=CARTESIAN_POINT('',(-15.8,-10.8786153175179,-2.20583969804343));
#26088=CARTESIAN_POINT('',(-24.9,-10.8786153175179,-2.20583969804343));
#26089=CARTESIAN_POINT('',(-15.8,-9.60550277460058,-5.56276158460351));
#26090=CARTESIAN_POINT('Origin',(-15.8,0.,0.));
#26091=CARTESIAN_POINT('',(-40.3,-9.60550277460058,-5.56276158460351));
#26092=CARTESIAN_POINT('',(-24.9,-9.60550277460058,-5.56276158460351));
#26093=CARTESIAN_POINT('',(-40.3,-8.60743066216474,-7.00871867005847));
#26094=CARTESIAN_POINT('Origin',(-40.3,0.,0.));
#26095=CARTESIAN_POINT('',(-15.8,-8.60743066216474,-7.00871867005847));
#26096=CARTESIAN_POINT('',(-24.9,-8.60743066216474,-7.00871867005847));
#26097=CARTESIAN_POINT('',(-15.8,-5.92010610227855,-9.38948048284698));
#26098=CARTESIAN_POINT('Origin',(-15.8,0.,0.));
#26099=CARTESIAN_POINT('',(-40.3,-5.92010610227855,-9.38948048284698));
#26100=CARTESIAN_POINT('',(-24.9,-5.92010610227855,-9.38948048284698));
#26101=CARTESIAN_POINT('',(-40.3,-4.36438737289401,-10.2059846589794));
#26102=CARTESIAN_POINT('Origin',(-40.3,0.,0.));
#26103=CARTESIAN_POINT('',(-15.8,-4.36438737289401,-10.2059846589794));
#26104=CARTESIAN_POINT('',(-24.9,-4.36438737289401,-10.2059846589794));
#26105=CARTESIAN_POINT('',(-15.8,-0.878484466937174,-11.0651825579766));
#26106=CARTESIAN_POINT('Origin',(-15.8,0.,0.));
#26107=CARTESIAN_POINT('',(-24.9,-0.878484466937175,-11.0651825579766));
#26108=CARTESIAN_POINT('Origin',(-40.3,0.,0.));
#26109=CARTESIAN_POINT('Origin',(-40.3,0.,0.));
#26110=CARTESIAN_POINT('Origin',(-40.3,0.,0.));
#26111=CARTESIAN_POINT('Origin',(-40.3,0.,0.));
#26112=CARTESIAN_POINT('',(-40.3,6.68001820616131,8.86495103005952));
#26113=CARTESIAN_POINT('Origin',(-40.3,0.,0.));
#26114=CARTESIAN_POINT('',(-15.8,6.68001820616131,8.86495103005952));
#26115=CARTESIAN_POINT('',(-24.9,6.68001820616131,8.86495103005952));
#26116=CARTESIAN_POINT('',(-15.8,3.50102881923381,10.5334133692215));
#26117=CARTESIAN_POINT('Origin',(-15.8,0.,0.));
#26118=CARTESIAN_POINT('',(-40.3,3.50102881923381,10.5334133692215));
#26119=CARTESIAN_POINT('',(-24.9,3.50102881923381,10.5334133692215));
#26120=CARTESIAN_POINT('',(-40.3,1.79511420941674,10.9538835567642));
#26121=CARTESIAN_POINT('Origin',(-40.3,0.,0.));
#26122=CARTESIAN_POINT('',(-15.8,1.79511420941674,10.9538835567642));
#26123=CARTESIAN_POINT('',(-24.9,1.79511420941674,10.9538835567642));
#26124=CARTESIAN_POINT('',(-15.8,-1.79511420941674,10.9538835567642));
#26125=CARTESIAN_POINT('Origin',(-15.8,0.,0.));
#26126=CARTESIAN_POINT('',(-40.3,-1.79511420941674,10.9538835567642));
#26127=CARTESIAN_POINT('',(-24.9,-1.79511420941674,10.9538835567642));
#26128=CARTESIAN_POINT('',(-40.3,-3.50102881923381,10.5334133692215));
#26129=CARTESIAN_POINT('Origin',(-40.3,0.,0.));
#26130=CARTESIAN_POINT('',(-15.8,-3.50102881923381,10.5334133692215));
#26131=CARTESIAN_POINT('',(-24.9,-3.50102881923381,10.5334133692215));
#26132=CARTESIAN_POINT('',(-15.8,-6.68001820616131,8.86495103005953));
#26133=CARTESIAN_POINT('Origin',(-15.8,0.,0.));
#26134=CARTESIAN_POINT('',(-40.3,-6.68001820616131,8.86495103005953));
#26135=CARTESIAN_POINT('',(-24.9,-6.68001820616131,8.86495103005953));
#26136=CARTESIAN_POINT('',(-40.3,-7.99512833736897,7.69986512018227));
#26137=CARTESIAN_POINT('Origin',(-40.3,0.,0.));
#26138=CARTESIAN_POINT('',(-15.8,-7.99512833736897,7.69986512018227));
#26139=CARTESIAN_POINT('',(-24.9,-7.99512833736897,7.69986512018227));
#26140=CARTESIAN_POINT('',(-15.8,-10.0346105348206,4.74516505660943));
#26141=CARTESIAN_POINT('Origin',(-15.8,0.,0.));
#26142=CARTESIAN_POINT('',(-40.3,-10.0346105348206,4.74516505660943));
#26143=CARTESIAN_POINT('',(-24.9,-10.0346105348206,4.74516505660943));
#26144=CARTESIAN_POINT('',(-40.3,-10.6576403051544,3.10237056554324));
#26145=CARTESIAN_POINT('Origin',(-40.3,0.,0.));
#26146=CARTESIAN_POINT('',(-15.8,-10.6576403051544,3.10237056554324));
#26147=CARTESIAN_POINT('',(-24.9,-10.6576403051544,3.10237056554324));
#26148=CARTESIAN_POINT('Origin',(-15.8,0.,0.));
#26149=CARTESIAN_POINT('Origin',(-24.9,-1.06736253355198,-10.7970534673528));
#26150=CARTESIAN_POINT('',(-16.2963973586152,-1.25624060016679,-10.5289243767289));
#26151=CARTESIAN_POINT('',(-24.9,-1.25624060016679,-10.5289243767289));
#26152=CARTESIAN_POINT('Ctrl Pts',(-15.8,-0.878484466937174,-11.0651825579766));
#26153=CARTESIAN_POINT('Ctrl Pts',(-15.967063448461,-1.00353264079959,-10.8876656353247));
#26154=CARTESIAN_POINT('Ctrl Pts',(-16.1329130514351,-1.1296182708827,-10.7086759519759));
#26155=CARTESIAN_POINT('Ctrl Pts',(-16.2963973586152,-1.25624060016679,
-10.5289243767289));
#26156=CARTESIAN_POINT('Origin',(-24.9,-4.07253834918427,-10.0563441542803));
#26157=CARTESIAN_POINT('',(-41.2927947172303,-3.78068932547453,-9.90670364958125));
#26158=CARTESIAN_POINT('Ctrl Pts',(-40.3,-4.36438737289401,-10.2059846589794));
#26159=CARTESIAN_POINT('Ctrl Pts',(-40.8162222946027,-4.06586327837569,
-10.0529216279618));
#26160=CARTESIAN_POINT('Ctrl Pts',(-41.2927947172303,-3.78068932547453,
-9.90670364958125));
#26161=CARTESIAN_POINT('',(-16.2963973586152,-3.78068932547453,-9.90670364958125));
#26162=CARTESIAN_POINT('',(-24.9,-3.78068932547453,-9.90670364958125));
#26163=CARTESIAN_POINT('Ctrl Pts',(-16.2963973586152,-3.78068932547453,
-9.90670364958125));
#26164=CARTESIAN_POINT('Ctrl Pts',(-16.1329130514351,-3.97634255215008,
-10.0070214344879));
#26165=CARTESIAN_POINT('Ctrl Pts',(-15.9670634484608,-4.17116648646451,
-10.1069140141776));
#26166=CARTESIAN_POINT('Ctrl Pts',(-15.8,-4.36438737289401,-10.2059846589794));
#26167=CARTESIAN_POINT('Origin',(-16.05,0.,0.));
#26168=CARTESIAN_POINT('',(-16.3,-3.77982060122741,-9.90317909676165));
#26169=CARTESIAN_POINT('Ctrl Pts',(-16.2963973586152,-3.78068932547454,
-9.9067036495813));
#26170=CARTESIAN_POINT('Ctrl Pts',(-16.2981989900368,-3.7802548895498,-9.90494107374833));
#26171=CARTESIAN_POINT('Ctrl Pts',(-16.3000000000001,-3.77982060122742,
-9.9031790967617));
#26172=CARTESIAN_POINT('',(-16.3,-1.25537187591967,-10.5253998239093));
#26173=CARTESIAN_POINT('Origin',(-16.3,0.,0.));
#26174=CARTESIAN_POINT('Ctrl Pts',(-16.3,-1.25537187591968,-10.5253998239093));
#26175=CARTESIAN_POINT('Ctrl Pts',(-16.2981989900368,-1.25580616424205,
-10.527161800896));
#26176=CARTESIAN_POINT('Ctrl Pts',(-16.2963973586152,-1.25624060016679,
-10.5289243767289));
#26177=CARTESIAN_POINT('Origin',(-41.3,-1.44204264379554,-11.2827529004882));
#26178=CARTESIAN_POINT('',(-16.3,-1.03520601450669,-9.63215181086392));
#26179=CARTESIAN_POINT('',(-16.3,-1.44204264379554,-11.2827529004882));
#26180=CARTESIAN_POINT('',(-40.8,-1.03520601450669,-9.63215181086392));
#26181=CARTESIAN_POINT('',(-41.3,-1.03520601450669,-9.63215181086392));
#26182=CARTESIAN_POINT('',(-41.3,-0.915548182362911,-9.1466809021509));
#26183=CARTESIAN_POINT('',(-40.625,-1.07708625575701,-9.80206662891349));
#26184=CARTESIAN_POINT('',(-41.3,0.213632391448158,-4.56541522611503));
#26185=CARTESIAN_POINT('Origin',(-16.3,-2.50084869180498,-10.1463419921022));
#26186=CARTESIAN_POINT('',(-16.3,-3.55965473981442,-9.00993108371627));
#26187=CARTESIAN_POINT('',(-16.3,-3.55965473981442,-9.00993108371627));
#26188=CARTESIAN_POINT('',(-16.3,-1.03520601450669,-9.63215181086392));
#26189=CARTESIAN_POINT('Origin',(-41.3,-3.55965473981442,-9.00993108371627));
#26190=CARTESIAN_POINT('',(-41.3,-3.77982060122741,-9.90317909676164));
#26191=CARTESIAN_POINT('Ctrl Pts',(-41.3,-3.77982060122741,-9.90317909676164));
#26192=CARTESIAN_POINT('Ctrl Pts',(-41.2963979800735,-3.78025488954978,
-9.90494107374827));
#26193=CARTESIAN_POINT('Ctrl Pts',(-41.2927947172303,-3.78068932547453,
-9.90670364958125));
#26194=CARTESIAN_POINT('',(-41.3,-3.43999690767065,-8.52446017500325));
#26195=CARTESIAN_POINT('',(-41.3,-2.10739801921515,-3.11789395415524));
#26196=CARTESIAN_POINT('',(-40.8,-3.55965473981442,-9.00993108371627));
#26197=CARTESIAN_POINT('',(-41.05,-3.49982582374253,-8.76719562935976));
#26198=CARTESIAN_POINT('',(-41.3,-3.55965473981442,-9.00993108371627));
#26199=CARTESIAN_POINT('Origin',(-24.9,-5.96274352296443,-9.06428794965443));
#26200=CARTESIAN_POINT('',(-16.2963973586152,-6.0053809436503,-8.73909541646189));
#26201=CARTESIAN_POINT('',(-41.2927947172303,-6.0053809436503,-8.73909541646189));
#26202=CARTESIAN_POINT('',(-24.9,-6.0053809436503,-8.73909541646189));
#26203=CARTESIAN_POINT('Ctrl Pts',(-41.2927947172303,-6.0053809436503,-8.73909541646189));
#26204=CARTESIAN_POINT('Ctrl Pts',(-40.8162222946065,-5.96371871143227,
-9.05685025752629));
#26205=CARTESIAN_POINT('Ctrl Pts',(-40.3,-5.92010610227855,-9.38948048284697));
#26206=CARTESIAN_POINT('Ctrl Pts',(-15.8,-5.92010610227855,-9.38948048284698));
#26207=CARTESIAN_POINT('Ctrl Pts',(-15.967063448461,-5.94833453393571,-9.17418427001376));
#26208=CARTESIAN_POINT('Ctrl Pts',(-16.1329130514352,-5.97679716143211,
-8.95710186240145));
#26209=CARTESIAN_POINT('Ctrl Pts',(-16.2963973586152,-6.0053809436503,-8.73909541646189));
#26210=CARTESIAN_POINT('Origin',(-24.9,-8.27946977552996,-7.01184758754715));
#26211=CARTESIAN_POINT('',(-41.2927947172303,-7.95150888889516,-7.01497650503582));
#26212=CARTESIAN_POINT('Ctrl Pts',(-40.3,-8.60743066216474,-7.00871867005847));
#26213=CARTESIAN_POINT('Ctrl Pts',(-40.816222294603,-8.27196876657345,-7.01191915107519));
#26214=CARTESIAN_POINT('Ctrl Pts',(-41.2927947172303,-7.95150888889516,
-7.01497650503582));
#26215=CARTESIAN_POINT('',(-16.2963973586152,-7.95150888889517,-7.01497650503582));
#26216=CARTESIAN_POINT('',(-24.9,-7.95150888889517,-7.01497650503582));
#26217=CARTESIAN_POINT('Ctrl Pts',(-16.2963973586152,-7.95150888889517,
-7.01497650503582));
#26218=CARTESIAN_POINT('Ctrl Pts',(-16.1329130514351,-8.17137121660771,
-7.01287890404035));
#26219=CARTESIAN_POINT('Ctrl Pts',(-15.9670634484609,-8.39030163968482,
-7.01079019389995));
#26220=CARTESIAN_POINT('Ctrl Pts',(-15.8,-8.60743066216474,-7.00871867005847));
#26221=CARTESIAN_POINT('Origin',(-16.05,0.,0.));
#26222=CARTESIAN_POINT('',(-16.3,-7.94910173040956,-7.01225938479173));
#26223=CARTESIAN_POINT('Ctrl Pts',(-16.2963973586152,-7.95150888889512,
-7.01497650503579));
#26224=CARTESIAN_POINT('Ctrl Pts',(-16.2981989900367,-7.95030510515574,
-7.01361771408482));
#26225=CARTESIAN_POINT('Ctrl Pts',(-16.3,-7.94910173040954,-7.01225938479171));
#26226=CARTESIAN_POINT('',(-16.3,-6.0029737851647,-8.7363782962178));
#26227=CARTESIAN_POINT('Origin',(-16.3,0.,0.));
#26228=CARTESIAN_POINT('Ctrl Pts',(-16.3,-6.00297378516469,-8.73637829621777));
#26229=CARTESIAN_POINT('Ctrl Pts',(-16.2981989900367,-6.0041771599109,-8.73773662551088));
#26230=CARTESIAN_POINT('Ctrl Pts',(-16.2963973586151,-6.00538094365029,
-8.73909541646186));
#26231=CARTESIAN_POINT('Origin',(-41.3,-6.52022206549856,-9.32023091004648));
#26232=CARTESIAN_POINT('',(-16.3,-5.39291354648921,-8.0477626381556));
#26233=CARTESIAN_POINT('',(-16.3,-6.52022206549856,-9.32023091004648));
#26234=CARTESIAN_POINT('',(-40.8,-5.39291354648921,-8.0477626381556));
#26235=CARTESIAN_POINT('',(-41.3,-5.39291354648921,-8.0477626381556));
#26236=CARTESIAN_POINT('',(-41.3,-5.06135221736881,-7.67350726407005));
#26237=CARTESIAN_POINT('',(-40.625,-5.50896001168135,-8.17875201908555));
#26238=CARTESIAN_POINT('',(-41.3,-6.0029737851647,-8.73637829621779));
#26239=CARTESIAN_POINT('',(-41.3,-0.443001249114668,-2.46046666651991));
#26240=CARTESIAN_POINT('Ctrl Pts',(-41.2927947172303,-6.0053809436503,-8.73909541646189));
#26241=CARTESIAN_POINT('Ctrl Pts',(-41.2963979800734,-6.00417715991092,
-8.73773662551092));
#26242=CARTESIAN_POINT('Ctrl Pts',(-41.3,-6.0029737851647,-8.73637829621779));
#26243=CARTESIAN_POINT('Origin',(-16.3,-6.92963177861631,-7.821937318388));
#26244=CARTESIAN_POINT('',(-16.3,-7.33904149173407,-6.32364372672953));
#26245=CARTESIAN_POINT('',(-16.3,-7.33904149173407,-6.32364372672953));
#26246=CARTESIAN_POINT('',(-16.3,-5.39291354648921,-8.0477626381556));
#26247=CARTESIAN_POINT('Origin',(-41.3,-7.33904149173407,-6.32364372672953));
#26248=CARTESIAN_POINT('',(-41.3,-7.94910173040956,-7.01225938479172));
#26249=CARTESIAN_POINT('Ctrl Pts',(-41.3,-7.94910173040956,-7.01225938479172));
#26250=CARTESIAN_POINT('Ctrl Pts',(-41.2963979800735,-7.95030510515576,
-7.01361771408483));
#26251=CARTESIAN_POINT('Ctrl Pts',(-41.2927947172303,-7.95150888889516,
-7.01497650503582));
#26252=CARTESIAN_POINT('',(-41.3,-7.00748016261367,-5.94938835264399));
#26253=CARTESIAN_POINT('',(-41.3,-1.82547493485485,-0.100113619148405));
#26254=CARTESIAN_POINT('',(-40.8,-7.33904149173407,-6.32364372672953));
#26255=CARTESIAN_POINT('',(-41.05,-7.17326082717387,-6.13651603968676));
#26256=CARTESIAN_POINT('',(-41.3,-7.33904149173407,-6.32364372672953));
#26257=CARTESIAN_POINT('Origin',(-41.05,4.65,9.35));
#26258=CARTESIAN_POINT('',(-41.3,-1.3,9.1));
#26259=CARTESIAN_POINT('',(-40.8,-1.3,9.6));
#26260=CARTESIAN_POINT('',(-40.625,-1.3,9.775));
#26261=CARTESIAN_POINT('',(-40.8,1.3,9.6));
#26262=CARTESIAN_POINT('',(-40.8,4.65,9.6));
#26263=CARTESIAN_POINT('',(-41.3,1.3,9.1));
#26264=CARTESIAN_POINT('',(-41.05,1.3,9.35));
#26265=CARTESIAN_POINT('',(-41.3,4.65,9.1));
#26266=CARTESIAN_POINT('Origin',(-41.3,-1.3,9.6));
#26267=CARTESIAN_POINT('',(-16.3,-1.3,9.6));
#26268=CARTESIAN_POINT('',(-41.3,-1.3,9.6));
#26269=CARTESIAN_POINT('',(-16.3,1.3,9.6));
#26270=CARTESIAN_POINT('',(-16.3,-1.3,9.6));
#26271=CARTESIAN_POINT('',(-41.3,1.3,9.6));
#26272=CARTESIAN_POINT('Origin',(-41.05,-0.765336496446259,10.1578510226473));
#26273=CARTESIAN_POINT('',(-41.3,-5.38007369894747,7.45350970978731));
#26274=CARTESIAN_POINT('',(-40.8,-5.61243528496935,7.89623772261392));
#26275=CARTESIAN_POINT('',(-40.625,-5.69376184007701,8.05119252710323));
#26276=CARTESIAN_POINT('',(-40.8,-3.310249618271,9.10451796992771));
#26277=CARTESIAN_POINT('',(-40.8,-0.8815172894572,10.3792150290606));
#26278=CARTESIAN_POINT('',(-41.3,-3.07788803224912,8.66178995710111));
#26279=CARTESIAN_POINT('',(-41.05,-3.19406882526006,8.88315396351441));
#26280=CARTESIAN_POINT('',(-41.3,-0.649155703435317,9.93648701623395));
#26281=CARTESIAN_POINT('Origin',(-41.3,-5.61243528496935,7.89623772261392));
#26282=CARTESIAN_POINT('',(-16.3,-5.61243528496935,7.89623772261392));
#26283=CARTESIAN_POINT('',(-41.3,-5.61243528496935,7.89623772261392));
#26284=CARTESIAN_POINT('',(-16.3,-3.310249618271,9.10451796992771));
#26285=CARTESIAN_POINT('',(-16.3,-5.61243528496935,7.89623772261392));
#26286=CARTESIAN_POINT('',(-41.3,-3.310249618271,9.10451796992771));
#26287=CARTESIAN_POINT('Origin',(-41.05,-6.35384418214366,7.25425891222178));
#26288=CARTESIAN_POINT('',(-41.3,-8.22763735038278,4.09951016959177));
#26289=CARTESIAN_POINT('',(-40.8,-8.6391292833296,4.38354254295734));
#26290=CARTESIAN_POINT('',(-40.625,-8.783151459861,4.4829538736353));
#26291=CARTESIAN_POINT('',(-40.8,-7.1621609418286,6.52330059428085));
#26292=CARTESIAN_POINT('',(-40.8,-6.55959014861707,7.39627509890457));
#26293=CARTESIAN_POINT('',(-41.3,-6.75066900888177,6.23926822091527));
#26294=CARTESIAN_POINT('',(-41.05,-6.95641497535519,6.38128440759806));
#26295=CARTESIAN_POINT('',(-41.3,-6.14809821567024,7.11224272553899));
#26296=CARTESIAN_POINT('Origin',(-41.3,-8.6391292833296,4.38354254295734));
#26297=CARTESIAN_POINT('',(-16.3,-8.6391292833296,4.38354254295734));
#26298=CARTESIAN_POINT('',(-41.3,-8.6391292833296,4.38354254295734));
#26299=CARTESIAN_POINT('',(-16.3,-7.1621609418286,6.52330059428085));
#26300=CARTESIAN_POINT('',(-16.3,-8.6391292833296,4.38354254295734));
#26301=CARTESIAN_POINT('',(-41.3,-7.1621609418286,6.52330059428085));
#26302=CARTESIAN_POINT('Origin',(-41.05,-9.2831726311618,1.11594370258557));
#26303=CARTESIAN_POINT('',(-41.3,-9.19034843862421,-0.193637746004029));
#26304=CARTESIAN_POINT('',(-40.8,-9.68670287567324,-0.133369405876367));
#26305=CARTESIAN_POINT('',(-40.625,-9.8604269286404,-0.112275486831686));
#26306=CARTESIAN_POINT('',(-40.8,-9.3733075070094,2.44767366677857));
#26307=CARTESIAN_POINT('',(-40.8,-9.53134984968631,1.1460778726494));
#26308=CARTESIAN_POINT('',(-41.3,-8.87695306996037,2.38740532665091));
#26309=CARTESIAN_POINT('',(-41.05,-9.12513028848489,2.41753949671474));
#26310=CARTESIAN_POINT('',(-41.3,-9.03499541263729,1.08580953252174));
#26311=CARTESIAN_POINT('Origin',(-41.3,-9.68670287567324,-0.133369405876367));
#26312=CARTESIAN_POINT('',(-16.3,-9.68670287567324,-0.133369405876367));
#26313=CARTESIAN_POINT('',(-41.3,-9.68670287567324,-0.133369405876367));
#26314=CARTESIAN_POINT('',(-16.3,-9.3733075070094,2.44767366677857));
#26315=CARTESIAN_POINT('',(-16.3,-9.68670287567324,-0.133369405876367));
#26316=CARTESIAN_POINT('',(-41.3,-9.3733075070094,2.44767366677857));
#26317=CARTESIAN_POINT('Origin',(-41.05,-7.8454621751844,-5.68059129593133));
#26318=CARTESIAN_POINT('',(-41.3,-8.04766145528198,-4.44242558757811));
#26319=CARTESIAN_POINT('',(-40.8,-8.51516957662469,-4.61972803109938));
#26320=CARTESIAN_POINT('',(-40.625,-8.67879741909464,-4.68178388633183));
#26321=CARTESIAN_POINT('',(-40.8,-9.43714228293528,-2.1886858001173));
#26322=CARTESIAN_POINT('',(-40.8,-8.07921623585575,-5.76924251769197));
#26323=CARTESIAN_POINT('',(-41.3,-8.96963416159257,-2.01138335659603));
#26324=CARTESIAN_POINT('',(-41.05,-9.20338822226393,-2.10003457835667));
#26325=CARTESIAN_POINT('',(-41.3,-7.61170811451305,-5.5919400741707));
#26326=CARTESIAN_POINT('Origin',(-41.3,-8.51516957662469,-4.61972803109938));
#26327=CARTESIAN_POINT('',(-16.3,-8.51516957662469,-4.61972803109938));
#26328=CARTESIAN_POINT('',(-41.3,-8.51516957662469,-4.61972803109938));
#26329=CARTESIAN_POINT('',(-16.3,-9.43714228293528,-2.1886858001173));
#26330=CARTESIAN_POINT('',(-16.3,-8.51516957662469,-4.61972803109938));
#26331=CARTESIAN_POINT('',(-41.3,-9.43714228293528,-2.1886858001173));
#26332=CARTESIAN_POINT('Origin',(-41.05,-2.74424266556362,-10.0602837396162));
#26333=CARTESIAN_POINT('',(-40.8,-2.91002333012382,-10.2474114266589));
#26334=CARTESIAN_POINT('',(-41.3,-2.57846200100342,-9.87315605257338));
#26335=CARTESIAN_POINT('Origin',(-41.3,-5.39291354648921,-8.0477626381556));
#26336=CARTESIAN_POINT('Origin',(-41.05,3.38996918821927,-10.4653775806365));
#26337=CARTESIAN_POINT('',(-40.8,3.33014027214738,-10.708113034993));
#26338=CARTESIAN_POINT('',(-41.3,3.44979810429116,-10.22264212628));
#26339=CARTESIAN_POINT('Origin',(-41.3,-1.03520601450669,-9.63215181086392));
#26340=CARTESIAN_POINT('Origin',(-41.05,7.8651721103966,-7.69123440523069));
#26341=CARTESIAN_POINT('',(-40.8,7.92500102646849,-7.9339698595872));
#26342=CARTESIAN_POINT('',(-41.3,7.80534319432471,-7.44849895087418));
#26343=CARTESIAN_POINT('Origin',(-41.3,3.55965473981442,-9.00993108371628));
#26344=CARTESIAN_POINT('',(-16.3,3.55965473981442,-9.00993108371628));
#26345=CARTESIAN_POINT('Origin',(-41.05,9.65615104353926,-3.93686725118344));
#26346=CARTESIAN_POINT('',(-40.8,9.82193170809946,-4.12399493822621));
#26347=CARTESIAN_POINT('',(-41.3,9.49037037897906,-3.74973956414066));
#26348=CARTESIAN_POINT('Origin',(-41.3,7.33904149173406,-6.32364372672954));
#26349=CARTESIAN_POINT('Origin',(-41.05,9.63934156303286,-0.950520091764082));
#26350=CARTESIAN_POINT('',(-40.8,9.87309562370421,-1.03917131352472));
#26351=CARTESIAN_POINT('',(-41.3,9.40558750236151,-0.861868870003448));
#26352=CARTESIAN_POINT('Origin',(-41.3,9.43714228293528,-2.18868580011731));
#26353=CARTESIAN_POINT('Origin',(-41.05,9.28048331447181,1.13809221818897));
#26354=CARTESIAN_POINT('',(-40.8,9.52866053299632,1.16822638825281));
#26355=CARTESIAN_POINT('',(-41.3,9.03230609594729,1.10795804812514));
#26356=CARTESIAN_POINT('Origin',(-41.3,9.3733075070094,2.44767366677856));
#26357=CARTESIAN_POINT('Origin',(-41.05,9.03595411006772,3.36855185165083));
#26358=CARTESIAN_POINT('',(-40.8,9.24170007654113,3.51056803833362));
#26359=CARTESIAN_POINT('',(-41.3,8.8302081435943,3.22653566496804));
#26360=CARTESIAN_POINT('Origin',(-41.3,7.1621609418286,6.52330059428085));
#26361=CARTESIAN_POINT('Origin',(-24.9,-9.49213183011501,-5.25500329920184));
#26362=CARTESIAN_POINT('',(-16.2963973586152,-9.37876088562945,-4.94724501380016));
#26363=CARTESIAN_POINT('',(-41.2927947172303,-9.37876088562945,-4.94724501380016));
#26364=CARTESIAN_POINT('',(-24.9,-9.37876088562945,-4.94724501380016));
#26365=CARTESIAN_POINT('Ctrl Pts',(-41.2927947172303,-9.37876088562945,
-4.94724501380016));
#26366=CARTESIAN_POINT('Ctrl Pts',(-40.8162222946069,-9.48953884874146,
-5.24796435721168));
#26367=CARTESIAN_POINT('Ctrl Pts',(-40.3,-9.60550277460057,-5.5627615846035));
#26368=CARTESIAN_POINT('Ctrl Pts',(-15.8,-9.60550277460058,-5.56276158460351));
#26369=CARTESIAN_POINT('Ctrl Pts',(-15.9670634484609,-9.53044467054936,
-5.35900784934866));
#26370=CARTESIAN_POINT('Ctrl Pts',(-16.1329130514351,-9.45476385051144,
-5.15356368093011));
#26371=CARTESIAN_POINT('Ctrl Pts',(-16.2963973586152,-9.37876088562945,
-4.94724501380016));
#26372=CARTESIAN_POINT('Origin',(-24.9,-10.589674454729,-2.36102124043076));
#26373=CARTESIAN_POINT('',(-41.2927947172303,-10.30073359194,-2.51620278281808));
#26374=CARTESIAN_POINT('Ctrl Pts',(-40.3,-10.8786153175179,-2.20583969804344));
#26375=CARTESIAN_POINT('Ctrl Pts',(-40.8162222946029,-10.5830658983798,
-2.36457049946365));
#26376=CARTESIAN_POINT('Ctrl Pts',(-41.2927947172303,-10.30073359194,-2.51620278281808));
#26377=CARTESIAN_POINT('',(-16.2963973586152,-10.30073359194,-2.51620278281808));
#26378=CARTESIAN_POINT('',(-24.9,-10.30073359194,-2.51620278281808));
#26379=CARTESIAN_POINT('Ctrl Pts',(-16.2963973586152,-10.30073359194,-2.51620278281808));
#26380=CARTESIAN_POINT('Ctrl Pts',(-16.1329130514352,-10.4944372110389,
-2.41217033102977));
#26381=CARTESIAN_POINT('Ctrl Pts',(-15.9670634484611,-10.6873198013493,
-2.30857882938089));
#26382=CARTESIAN_POINT('Ctrl Pts',(-15.8,-10.8786153175179,-2.20583969804343));
#26383=CARTESIAN_POINT('Origin',(-16.05,0.,0.));
#26384=CARTESIAN_POINT('',(-16.3,-10.2973394502156,-2.51491555465257));
#26385=CARTESIAN_POINT('Ctrl Pts',(-16.2963973586152,-10.3007335919401,
-2.51620278281809));
#26386=CARTESIAN_POINT('Ctrl Pts',(-16.2981989900368,-10.2990362327336,
-2.51555905938076));
#26387=CARTESIAN_POINT('Ctrl Pts',(-16.3000000000001,-10.2973394502156,
-2.51491555465257));
#26388=CARTESIAN_POINT('',(-16.3,-9.37536674390501,-4.94595778563465));
#26389=CARTESIAN_POINT('Origin',(-16.3,0.,0.));
#26390=CARTESIAN_POINT('Ctrl Pts',(-16.3000000000001,-9.37536674390505,
-4.94595778563467));
#26391=CARTESIAN_POINT('Ctrl Pts',(-16.2981989900368,-9.37706352642298,
-4.94660129036286));
#26392=CARTESIAN_POINT('Ctrl Pts',(-16.2963973586152,-9.37876088562949,
-4.94724501380019));
#26393=CARTESIAN_POINT('Origin',(-41.3,-10.1046971891899,-5.22255633907169));
#26394=CARTESIAN_POINT('',(-16.3,-10.1046971891899,-5.22255633907169));
#26395=CARTESIAN_POINT('',(-41.3,-9.375366743905,-4.94595778563464));
#26396=CARTESIAN_POINT('',(-41.3,-0.18830193536388,-1.46176368294326));
#26397=CARTESIAN_POINT('Ctrl Pts',(-41.2927947172303,-9.37876088562945,
-4.94724501380016));
#26398=CARTESIAN_POINT('Ctrl Pts',(-41.2963979800734,-9.37706352642294,
-4.94660129036284));
#26399=CARTESIAN_POINT('Ctrl Pts',(-41.3,-9.375366743905,-4.94595778563464));
#26400=CARTESIAN_POINT('Origin',(-16.3,-9.77091973606259,-3.7056210695945));
#26401=CARTESIAN_POINT('',(-16.3,-9.43714228293528,-2.1886858001173));
#26402=CARTESIAN_POINT('Origin',(-41.3,-9.43714228293528,-2.1886858001173));
#26403=CARTESIAN_POINT('',(-41.3,-10.2973394502156,-2.51491555465256));
#26404=CARTESIAN_POINT('Ctrl Pts',(-41.3,-10.2973394502156,-2.51491555465256));
#26405=CARTESIAN_POINT('Ctrl Pts',(-41.2963979800735,-10.2990362327335,
-2.51555905938075));
#26406=CARTESIAN_POINT('Ctrl Pts',(-41.2927947172303,-10.30073359194,-2.51620278281808));
#26407=CARTESIAN_POINT('',(-41.3,-0.315510835391869,1.27069270202498));
#26408=CARTESIAN_POINT('Origin',(-24.9,-10.8469871275755,-0.241860722557092));
#26409=CARTESIAN_POINT('',(-16.2963973586152,-10.6035797350322,-0.0220403992424092));
#26410=CARTESIAN_POINT('',(-41.2927947172303,-10.6035797350322,-0.0220403992424095));
#26411=CARTESIAN_POINT('',(-24.9,-10.6035797350322,-0.0220403992424092));
#26412=CARTESIAN_POINT('Ctrl Pts',(-41.2927947172303,-10.6035797350322,
-0.0220403992424095));
#26413=CARTESIAN_POINT('Ctrl Pts',(-40.8162222946062,-10.8414199971447,
-0.236833067486949));
#26414=CARTESIAN_POINT('Ctrl Pts',(-40.3,-11.0903945201189,-0.461681045871771));
#26415=CARTESIAN_POINT('Ctrl Pts',(-15.8,-11.0903945201189,-0.461681045871777));
#26416=CARTESIAN_POINT('Ctrl Pts',(-15.967063448461,-10.9292447874491,-0.316147313443195));
#26417=CARTESIAN_POINT('Ctrl Pts',(-16.1329130514351,-10.7667580836948,
-0.169406167332626));
#26418=CARTESIAN_POINT('Ctrl Pts',(-16.2963973586152,-10.6035797350322,
-0.0220403992424079));
#26419=CARTESIAN_POINT('Origin',(-24.9,-10.4739123357613,2.83068661947789));
#26420=CARTESIAN_POINT('',(-41.2927947172303,-10.2901843663683,2.55900267341253));
#26421=CARTESIAN_POINT('Ctrl Pts',(-40.3,-10.6576403051544,3.10237056554323));
#26422=CARTESIAN_POINT('Ctrl Pts',(-40.8162222946031,-10.4697101726372,
2.82447275741129));
#26423=CARTESIAN_POINT('Ctrl Pts',(-41.2927947172303,-10.2901843663683,
2.55900267341253));
#26424=CARTESIAN_POINT('',(-16.2963973586152,-10.2901843663683,2.55900267341253));
#26425=CARTESIAN_POINT('',(-24.9,-10.2901843663683,2.55900267341253));
#26426=CARTESIAN_POINT('Ctrl Pts',(-16.2963973586152,-10.2901843663683,
2.55900267341253));
#26427=CARTESIAN_POINT('Ctrl Pts',(-16.1329130514351,-10.4133541120997,
2.741137395016));
#26428=CARTESIAN_POINT('Ctrl Pts',(-15.967063448461,-10.5360017926907,2.92250012355862));
#26429=CARTESIAN_POINT('Ctrl Pts',(-15.8,-10.6576403051544,3.10237056554324));
#26430=CARTESIAN_POINT('Origin',(-16.05,0.,0.));
#26431=CARTESIAN_POINT('',(-16.3,-10.2865807983703,2.55856512103953));
#26432=CARTESIAN_POINT('Ctrl Pts',(-16.2963973586152,-10.2901843663683,
2.55900267341253));
#26433=CARTESIAN_POINT('Ctrl Pts',(-16.2981989900368,-10.2883822762335,
2.55878386005441));
#26434=CARTESIAN_POINT('Ctrl Pts',(-16.3000000000001,-10.2865807983703,
2.55856512103953));
#26435=CARTESIAN_POINT('',(-16.3,-10.5999761670341,-0.0224779516154086));
#26436=CARTESIAN_POINT('Origin',(-16.3,0.,0.));
#26437=CARTESIAN_POINT('Ctrl Pts',(-16.3000000000001,-10.5999761670342,
-0.022477951615407));
#26438=CARTESIAN_POINT('Ctrl Pts',(-16.2981989900368,-10.6017776448974,
-0.022259212600522));
#26439=CARTESIAN_POINT('Ctrl Pts',(-16.2963973586152,-10.6035797350322,
-0.022040399242408));
#26440=CARTESIAN_POINT('Origin',(-41.3,-11.3743079616399,0.0715429505576823));
#26441=CARTESIAN_POINT('',(-16.3,-11.3743079616399,0.0715429505576823));
#26442=CARTESIAN_POINT('',(-41.3,-10.5999761670341,-0.0224779516154098));
#26443=CARTESIAN_POINT('',(-41.3,-0.542507006806888,-1.24367580324692));
#26444=CARTESIAN_POINT('Ctrl Pts',(-41.2927947172303,-10.6035797350322,
-0.0220403992424095));
#26445=CARTESIAN_POINT('Ctrl Pts',(-41.2963979800735,-10.6017776448973,
-0.0222592126005259));
#26446=CARTESIAN_POINT('Ctrl Pts',(-41.3,-10.5999761670341,-0.0224779516154095));
#26447=CARTESIAN_POINT('Origin',(-16.3,-10.3738077343247,1.25960830866813));
#26448=CARTESIAN_POINT('',(-16.3,-9.3733075070094,2.44767366677857));
#26449=CARTESIAN_POINT('Origin',(-41.3,-9.3733075070094,2.44767366677857));
#26450=CARTESIAN_POINT('',(-41.3,-10.2865807983703,2.55856512103953));
#26451=CARTESIAN_POINT('Ctrl Pts',(-41.3,-10.2865807983703,2.55856512103953));
#26452=CARTESIAN_POINT('Ctrl Pts',(-41.2963979800734,-10.2883822762335,
2.55878386005442));
#26453=CARTESIAN_POINT('Ctrl Pts',(-41.2927947172303,-10.2901843663683,
2.55900267341253));
#26454=CARTESIAN_POINT('',(-41.3,0.614690904840299,1.23491109119099));
#26455=CARTESIAN_POINT('Origin',(-24.9,-9.71692839447407,4.8266892308878));
#26456=CARTESIAN_POINT('',(-16.2963973586152,-9.39924625412754,4.90821340516617));
#26457=CARTESIAN_POINT('',(-41.2927947172303,-9.39924625412754,4.90821340516618));
#26458=CARTESIAN_POINT('',(-24.9,-9.39924625412754,4.90821340516617));
#26459=CARTESIAN_POINT('Ctrl Pts',(-41.2927947172303,-9.39924625412754,
4.90821340516618));
#26460=CARTESIAN_POINT('Ctrl Pts',(-40.8162222946068,-9.70966247747601,
4.82855382385169));
#26461=CARTESIAN_POINT('Ctrl Pts',(-40.3,-10.0346105348206,4.74516505660943));
#26462=CARTESIAN_POINT('Ctrl Pts',(-15.8,-10.0346105348206,4.74516505660943));
#26463=CARTESIAN_POINT('Ctrl Pts',(-15.967063448461,-9.8242866352221,4.79913876198384));
#26464=CARTESIAN_POINT('Ctrl Pts',(-16.1329130514352,-9.61221779340458,
4.85356025763508));
#26465=CARTESIAN_POINT('Ctrl Pts',(-16.2963973586152,-9.39924625412754,
4.90821340516617));
#26466=CARTESIAN_POINT('Origin',(-24.9,-7.95870312499775,7.37391828833598));
#26467=CARTESIAN_POINT('',(-41.2927947172303,-7.92227791262653,7.04797145648968));
#26468=CARTESIAN_POINT('Ctrl Pts',(-40.3,-7.99512833736897,7.69986512018227));
#26469=CARTESIAN_POINT('Ctrl Pts',(-40.8162222946026,-7.95787002002895,
7.36646334415037));
#26470=CARTESIAN_POINT('Ctrl Pts',(-41.2927947172303,-7.92227791262653,
7.04797145648968));
#26471=CARTESIAN_POINT('',(-16.2963973586152,-7.92227791262653,7.04797145648968));
#26472=CARTESIAN_POINT('',(-24.9,-7.92227791262653,7.04797145648968));
#26473=CARTESIAN_POINT('Ctrl Pts',(-16.2963973586152,-7.92227791262653,
7.04797145648968));
#26474=CARTESIAN_POINT('Ctrl Pts',(-16.1329130514351,-7.94669708059969,
7.26648357815028));
#26475=CARTESIAN_POINT('Ctrl Pts',(-15.9670634484609,-7.9710127459125,7.48406951813532));
#26476=CARTESIAN_POINT('Ctrl Pts',(-15.8,-7.99512833736897,7.69986512018228));
#26477=CARTESIAN_POINT('Origin',(-16.05,0.,0.));
#26478=CARTESIAN_POINT('',(-16.3,-7.91929045235552,7.04590936155374));
#26479=CARTESIAN_POINT('Ctrl Pts',(-16.2963973586152,-7.92227791262651,
7.04797145648969));
#26480=CARTESIAN_POINT('Ctrl Pts',(-16.2981989900368,-7.92078392869575,
7.0469402338395));
#26481=CARTESIAN_POINT('Ctrl Pts',(-16.3,-7.91929045235552,7.04590936155376));
#26482=CARTESIAN_POINT('',(-16.3,-9.39625879385653,4.90615131023023));
#26483=CARTESIAN_POINT('Origin',(-16.3,0.,0.));
#26484=CARTESIAN_POINT('Ctrl Pts',(-16.3000000000001,-9.39625879385658,
4.90615131023027));
#26485=CARTESIAN_POINT('Ctrl Pts',(-16.2981989900368,-9.39775227019682,
4.90718218251601));
#26486=CARTESIAN_POINT('Ctrl Pts',(-16.2963973586152,-9.39924625412759,
4.9082134051662));
#26487=CARTESIAN_POINT('Origin',(-41.3,-10.0382018553488,5.34925261240031));
#26488=CARTESIAN_POINT('',(-16.3,-10.0382018553488,5.34925261240031));
#26489=CARTESIAN_POINT('',(-41.3,-9.39625879385652,4.90615131023023));
#26490=CARTESIAN_POINT('',(-41.3,-1.79864006238694,-0.338106249747072));
#26491=CARTESIAN_POINT('Ctrl Pts',(-41.2927947172303,-9.39924625412754,
4.90821340516618));
#26492=CARTESIAN_POINT('Ctrl Pts',(-41.2963979800734,-9.39775227019676,
4.90718218251598));
#26493=CARTESIAN_POINT('Ctrl Pts',(-41.3,-9.39625879385652,4.90615131023023));
#26494=CARTESIAN_POINT('Origin',(-16.3,-8.60018139858871,5.93627660334058));
#26495=CARTESIAN_POINT('',(-16.3,-7.1621609418286,6.52330059428085));
#26496=CARTESIAN_POINT('Origin',(-41.3,-7.1621609418286,6.52330059428085));
#26497=CARTESIAN_POINT('',(-41.3,-7.91929045235552,7.04590936155374));
#26498=CARTESIAN_POINT('Ctrl Pts',(-41.3,-7.91929045235552,7.04590936155374));
#26499=CARTESIAN_POINT('Ctrl Pts',(-41.2963979800734,-7.92078392869579,
7.0469402338395));
#26500=CARTESIAN_POINT('Ctrl Pts',(-41.2927947172303,-7.92227791262653,
7.04797145648968));
#26501=CARTESIAN_POINT('',(-41.3,0.377864565123671,1.31879676685495));
#26502=CARTESIAN_POINT('Origin',(-24.9,-6.36083846788016,8.78950284944722));
#26503=CARTESIAN_POINT('',(-16.2963973586152,-6.04165872959902,8.71405466883491));
#26504=CARTESIAN_POINT('',(-41.2927947172303,-6.04165872959902,8.71405466883491));
#26505=CARTESIAN_POINT('',(-24.9,-6.04165872959902,8.71405466883491));
#26506=CARTESIAN_POINT('Ctrl Pts',(-41.2927947172303,-6.04165872959902,
8.71405466883491));
#26507=CARTESIAN_POINT('Ctrl Pts',(-40.8162222946063,-6.35353829833592,
8.78777722452741));
#26508=CARTESIAN_POINT('Ctrl Pts',(-40.3,-6.6800182061613,8.86495103005952));
#26509=CARTESIAN_POINT('Ctrl Pts',(-15.8,-6.68001820616131,8.86495103005953));
#26510=CARTESIAN_POINT('Ctrl Pts',(-15.967063448461,-6.46870281035439,8.8149999829321));
#26511=CARTESIAN_POINT('Ctrl Pts',(-16.1329130514352,-6.25563424642735,
8.76463451932045));
#26512=CARTESIAN_POINT('Ctrl Pts',(-16.2963973586152,-6.04165872959902,
8.71405466883491));
#26513=CARTESIAN_POINT('Origin',(-24.9,-3.62025094106724,10.2278741426851));
#26514=CARTESIAN_POINT('',(-41.2927947172303,-3.73947306290067,9.9223349161487));
#26515=CARTESIAN_POINT('Ctrl Pts',(-40.3,-3.50102881923381,10.5334133692215));
#26516=CARTESIAN_POINT('Ctrl Pts',(-40.8162222946038,-3.62297774856226,
10.2208859542505));
#26517=CARTESIAN_POINT('Ctrl Pts',(-41.2927947172303,-3.73947306290067,
9.9223349161487));
#26518=CARTESIAN_POINT('',(-16.2963973586152,-3.73947306290067,9.9223349161487));
#26519=CARTESIAN_POINT('',(-24.9,-3.73947306290067,9.9223349161487));
#26520=CARTESIAN_POINT('Ctrl Pts',(-16.2963973586152,-3.73947306290067,
9.9223349161487));
#26521=CARTESIAN_POINT('Ctrl Pts',(-16.1329130514351,-3.65954751601581,
10.1271659441505));
#26522=CARTESIAN_POINT('Ctrl Pts',(-15.9670634484609,-3.57996074016283,
10.3311287789222));
#26523=CARTESIAN_POINT('Ctrl Pts',(-15.8,-3.50102881923381,10.5334133692215));
#26524=CARTESIAN_POINT('Origin',(-16.05,0.,0.));
#26525=CARTESIAN_POINT('',(-16.3,-3.737786101502,9.91912067974871));
#26526=CARTESIAN_POINT('Ctrl Pts',(-16.2963973586153,-3.7394730629007,9.92233491614877));
#26527=CARTESIAN_POINT('Ctrl Pts',(-16.2981989900368,-3.73862943888804,
9.92072752488807));
#26528=CARTESIAN_POINT('Ctrl Pts',(-16.3000000000001,-3.73778610150201,
9.91912067974877));
#26529=CARTESIAN_POINT('',(-16.3,-6.03997176820034,8.71084043243491));
#26530=CARTESIAN_POINT('Origin',(-16.3,0.,0.));
#26531=CARTESIAN_POINT('Ctrl Pts',(-16.3000000000001,-6.03997176820037,
8.71084043243496));
#26532=CARTESIAN_POINT('Ctrl Pts',(-16.2981989900368,-6.0408151055864,8.71244727757426));
#26533=CARTESIAN_POINT('Ctrl Pts',(-16.2963973586152,-6.04165872959905,
8.71405466883496));
#26534=CARTESIAN_POINT('Origin',(-41.3,-6.40246467744376,9.40151296622437));
#26535=CARTESIAN_POINT('',(-16.3,-6.40246467744376,9.40151296622437));
#26536=CARTESIAN_POINT('',(-41.3,-6.03997176820034,8.71084043243491));
#26537=CARTESIAN_POINT('',(-41.3,-2.63215033423403,2.21777917666555));
#26538=CARTESIAN_POINT('Ctrl Pts',(-41.2927947172303,-6.04165872959902,
8.71405466883491));
#26539=CARTESIAN_POINT('Ctrl Pts',(-41.2963979800735,-6.04081510558637,
8.71244727757421));
#26540=CARTESIAN_POINT('Ctrl Pts',(-41.3,-6.03997176820034,8.71084043243491));
#26541=CARTESIAN_POINT('Origin',(-16.3,-4.85635714785738,9.25301546807604));
#26542=CARTESIAN_POINT('',(-16.3,-3.310249618271,9.10451796992771));
#26543=CARTESIAN_POINT('Origin',(-41.3,-3.310249618271,9.10451796992771));
#26544=CARTESIAN_POINT('',(-41.3,-3.73778610150199,9.9191206797487));
#26545=CARTESIAN_POINT('Ctrl Pts',(-41.3,-3.73778610150199,9.9191206797487));
#26546=CARTESIAN_POINT('Ctrl Pts',(-41.2963979800734,-3.73862943888803,
9.92072752488801));
#26547=CARTESIAN_POINT('Ctrl Pts',(-41.2927947172303,-3.73947306290067,
9.9223349161487));
#26548=CARTESIAN_POINT('',(-41.3,0.0650500287015215,2.67342180217412));
#26549=CARTESIAN_POINT('Origin',(-24.9,-1.54755710470837,10.7387472901904));
#26550=CARTESIAN_POINT('',(-16.2963973586152,-1.3,10.5236110236165));
#26551=CARTESIAN_POINT('',(-41.2927947172303,-1.3,10.5236110236165));
#26552=CARTESIAN_POINT('',(-24.9,-1.3,10.5236110236165));
#26553=CARTESIAN_POINT('Ctrl Pts',(-41.2927947172303,-1.3,10.5236110236165));
#26554=CARTESIAN_POINT('Ctrl Pts',(-40.8162222946067,-1.54189506348343,
10.7338267672599));
#26555=CARTESIAN_POINT('Ctrl Pts',(-40.3,-1.79511420941673,10.9538835567642));
#26556=CARTESIAN_POINT('Ctrl Pts',(-15.8,-1.79511420941674,10.9538835567642));
#26557=CARTESIAN_POINT('Ctrl Pts',(-15.9670634484609,-1.63121712795427,
10.8114509400566));
#26558=CARTESIAN_POINT('Ctrl Pts',(-16.1329130514351,-1.4659602821588,10.6678366379258));
#26559=CARTESIAN_POINT('Ctrl Pts',(-16.2963973586152,-1.3,10.5236110236165));
#26560=CARTESIAN_POINT('Origin',(-24.9,1.54755710470837,10.7387472901904));
#26561=CARTESIAN_POINT('',(-41.2927947172303,1.3,10.5236110236165));
#26562=CARTESIAN_POINT('Ctrl Pts',(-40.3,1.79511420941673,10.9538835567642));
#26563=CARTESIAN_POINT('Ctrl Pts',(-40.8162222946033,1.5418950634852,10.7338267672615));
#26564=CARTESIAN_POINT('Ctrl Pts',(-41.2927947172303,1.3,10.5236110236165));
#26565=CARTESIAN_POINT('',(-16.2963973586152,1.3,10.5236110236165));
#26566=CARTESIAN_POINT('',(-24.9,1.3,10.5236110236165));
#26567=CARTESIAN_POINT('Ctrl Pts',(-16.2963973586152,1.3,10.5236110236165));
#26568=CARTESIAN_POINT('Ctrl Pts',(-16.1329130514351,1.46596028215881,10.6678366379258));
#26569=CARTESIAN_POINT('Ctrl Pts',(-15.9670634484609,1.63121712795429,10.8114509400566));
#26570=CARTESIAN_POINT('Ctrl Pts',(-15.8,1.79511420941674,10.9538835567642));
#26571=CARTESIAN_POINT('Origin',(-16.05,0.,0.));
#26572=CARTESIAN_POINT('',(-16.3,1.3,10.519980988576));
#26573=CARTESIAN_POINT('Ctrl Pts',(-16.2963973586153,1.3,10.5236110236166));
#26574=CARTESIAN_POINT('Ctrl Pts',(-16.2981989900368,1.3,10.521795697712));
#26575=CARTESIAN_POINT('Ctrl Pts',(-16.3000000000001,1.3,10.519980988576));
#26576=CARTESIAN_POINT('',(-16.3,-1.3,10.519980988576));
#26577=CARTESIAN_POINT('Origin',(-16.3,0.,0.));
#26578=CARTESIAN_POINT('Ctrl Pts',(-16.3,-1.3,10.519980988576));
#26579=CARTESIAN_POINT('Ctrl Pts',(-16.2981989900368,-1.3,10.521795697712));
#26580=CARTESIAN_POINT('Ctrl Pts',(-16.2963973586152,-1.3,10.5236110236166));
#26581=CARTESIAN_POINT('Origin',(-16.3,0.,10.45));
#26582=CARTESIAN_POINT('',(-16.3,1.3,9.6));
#26583=CARTESIAN_POINT('',(-16.3,-1.3,11.3));
#26584=CARTESIAN_POINT('Origin',(-41.3,1.3,9.6));
#26585=CARTESIAN_POINT('',(-41.3,1.3,10.519980988576));
#26586=CARTESIAN_POINT('Ctrl Pts',(-41.3,1.3,10.519980988576));
#26587=CARTESIAN_POINT('Ctrl Pts',(-41.2963979800735,1.3,10.521795697712));
#26588=CARTESIAN_POINT('Ctrl Pts',(-41.2927947172303,1.3,10.5236110236165));
#26589=CARTESIAN_POINT('',(-41.3,1.3,4.8));
#26590=CARTESIAN_POINT('Origin',(-40.8,0.,0.));
#26591=CARTESIAN_POINT('',(-41.2927947172303,3.73947306290068,9.9223349161487));
#26592=CARTESIAN_POINT('Ctrl Pts',(-41.2927947172303,3.73947306290068,9.92233491614871));
#26593=CARTESIAN_POINT('Ctrl Pts',(-40.8162222946065,3.62297774856297,10.2208859542487));
#26594=CARTESIAN_POINT('Ctrl Pts',(-40.3,3.50102881923382,10.5334133692215));
#26595=CARTESIAN_POINT('',(-41.3,3.737786101502,9.9191206797487));
#26596=CARTESIAN_POINT('Ctrl Pts',(-41.2927947172303,3.73947306290068,9.92233491614871));
#26597=CARTESIAN_POINT('Ctrl Pts',(-41.2963979800734,3.73862943888804,9.92072752488803));
#26598=CARTESIAN_POINT('Ctrl Pts',(-41.3,3.737786101502,9.9191206797487));
#26599=CARTESIAN_POINT('Origin',(-41.3,0.,0.));
#26600=CARTESIAN_POINT('Origin',(-41.05,7.92498682077222,6.40017665706777));
#26601=CARTESIAN_POINT('',(-41.3,3.07788803224913,8.66178995710111));
#26602=CARTESIAN_POINT('',(-40.8,3.31024961827101,9.10451796992771));
#26603=CARTESIAN_POINT('',(-40.625,3.39157617337867,9.25947277441703));
#26604=CARTESIAN_POINT('',(-40.8,5.61243528496936,7.89623772261391));
#26605=CARTESIAN_POINT('',(-40.8,8.04116761378316,6.62154066348107));
#26606=CARTESIAN_POINT('',(-41.3,5.38007369894747,7.45350970978731));
#26607=CARTESIAN_POINT('',(-41.05,5.49625449195841,7.67487371620061));
#26608=CARTESIAN_POINT('',(-41.3,7.80880602776127,6.17881265065447));
#26609=CARTESIAN_POINT('Origin',(-41.3,3.31024961827101,9.10451796992771));
#26610=CARTESIAN_POINT('',(-16.3,3.31024961827101,9.10451796992771));
#26611=CARTESIAN_POINT('',(-41.3,3.31024961827101,9.10451796992771));
#26612=CARTESIAN_POINT('',(-16.3,5.61243528496936,7.89623772261391));
#26613=CARTESIAN_POINT('',(-16.3,3.31024961827101,9.10451796992771));
#26614=CARTESIAN_POINT('',(-41.3,5.61243528496936,7.89623772261391));
#26615=CARTESIAN_POINT('Origin',(-24.9,3.62025094106725,10.2278741426851));
#26616=CARTESIAN_POINT('',(-16.2963973586152,3.73947306290068,9.9223349161487));
#26617=CARTESIAN_POINT('',(-24.9,3.73947306290068,9.9223349161487));
#26618=CARTESIAN_POINT('Ctrl Pts',(-15.8,3.50102881923381,10.5334133692215));
#26619=CARTESIAN_POINT('Ctrl Pts',(-15.9670634484609,3.57996074016282,10.3311287789223));
#26620=CARTESIAN_POINT('Ctrl Pts',(-16.1329130514351,3.65954751601581,10.1271659441505));
#26621=CARTESIAN_POINT('Ctrl Pts',(-16.2963973586152,3.73947306290068,9.9223349161487));
#26622=CARTESIAN_POINT('Origin',(-24.9,6.36083846788017,8.78950284944721));
#26623=CARTESIAN_POINT('',(-41.2927947172303,6.04165872959903,8.7140546688349));
#26624=CARTESIAN_POINT('Ctrl Pts',(-40.3,6.6800182061613,8.86495103005952));
#26625=CARTESIAN_POINT('Ctrl Pts',(-40.8162222946031,6.35353829833807,8.78777722452791));
#26626=CARTESIAN_POINT('Ctrl Pts',(-41.2927947172303,6.04165872959903,8.7140546688349));
#26627=CARTESIAN_POINT('',(-16.2963973586152,6.04165872959903,8.7140546688349));
#26628=CARTESIAN_POINT('',(-24.9,6.04165872959903,8.7140546688349));
#26629=CARTESIAN_POINT('Ctrl Pts',(-16.2963973586152,6.04165872959903,8.7140546688349));
#26630=CARTESIAN_POINT('Ctrl Pts',(-16.1329130514352,6.25563424642728,8.76463451932043));
#26631=CARTESIAN_POINT('Ctrl Pts',(-15.9670634484612,6.46870281035421,8.81499998293205));
#26632=CARTESIAN_POINT('Ctrl Pts',(-15.8,6.68001820616131,8.86495103005952));
#26633=CARTESIAN_POINT('Origin',(-16.05,0.,0.));
#26634=CARTESIAN_POINT('',(-16.3,6.03997176820035,8.71084043243491));
#26635=CARTESIAN_POINT('Ctrl Pts',(-16.2963973586152,6.04165872959901,8.71405466883492));
#26636=CARTESIAN_POINT('Ctrl Pts',(-16.2981989900368,6.04081510558637,8.71244727757422));
#26637=CARTESIAN_POINT('Ctrl Pts',(-16.3000000000001,6.03997176820034,8.71084043243492));
#26638=CARTESIAN_POINT('',(-16.3,3.737786101502,9.91912067974871));
#26639=CARTESIAN_POINT('Origin',(-16.3,0.,0.));
#26640=CARTESIAN_POINT('Ctrl Pts',(-16.3,3.73778610150202,9.9191206797487));
#26641=CARTESIAN_POINT('Ctrl Pts',(-16.2981989900367,3.73862943888804,9.92072752488799));
#26642=CARTESIAN_POINT('Ctrl Pts',(-16.2963973586152,3.73947306290069,9.92233491614868));
#26643=CARTESIAN_POINT('Origin',(-16.3,4.85635714785739,9.25301546807604));
#26644=CARTESIAN_POINT('',(-16.3,5.61243528496936,7.89623772261391));
#26645=CARTESIAN_POINT('',(-16.3,4.10027901074542,10.6097932135382));
#26646=CARTESIAN_POINT('Origin',(-41.3,5.61243528496936,7.89623772261391));
#26647=CARTESIAN_POINT('',(-41.3,6.03997176820034,8.7108404324349));
#26648=CARTESIAN_POINT('Ctrl Pts',(-41.3,6.03997176820034,8.7108404324349));
#26649=CARTESIAN_POINT('Ctrl Pts',(-41.2963979800734,6.04081510558637,8.7124472775742));
#26650=CARTESIAN_POINT('Ctrl Pts',(-41.2927947172303,6.04165872959903,8.7140546688349));
#26651=CARTESIAN_POINT('',(-41.3,4.5263924803217,5.8269560440967));
#26652=CARTESIAN_POINT('Origin',(-40.8,0.,0.));
#26653=CARTESIAN_POINT('Origin',(-41.3,0.,0.));
#26654=CARTESIAN_POINT('Origin',(-41.05,0.,0.));
#26655=CARTESIAN_POINT('',(-41.3,4.71489017671731E-16,3.85));
#26656=CARTESIAN_POINT('Origin',(-41.3,0.,0.));
#26657=CARTESIAN_POINT('',(-40.8,-4.10256677714363E-16,3.35));
#26658=CARTESIAN_POINT('',(-41.05,4.40872847693047E-16,3.6));
#26659=CARTESIAN_POINT('Origin',(-40.8,0.,0.));
#26660=CARTESIAN_POINT('Origin',(-41.3,0.,0.));
#26661=CARTESIAN_POINT('',(-27.3,-4.10256677714363E-16,3.35));
#26662=CARTESIAN_POINT('',(-41.3,-4.10256677714363E-16,3.35));
#26663=CARTESIAN_POINT('Origin',(-27.3,0.,0.));
#26664=CARTESIAN_POINT('Origin',(-41.3,10.6,0.));
#26665=CARTESIAN_POINT('',(-41.3,2.61922150986056,7.78787391321573));
#26666=CARTESIAN_POINT('Origin',(-41.3,0.,0.));
#26667=CARTESIAN_POINT('Origin',(-41.3,0.,0.));
#26668=CARTESIAN_POINT('Origin',(-41.3,0.,0.));
#26669=CARTESIAN_POINT('Origin',(-41.3,0.,0.));
#26670=CARTESIAN_POINT('Origin',(-41.3,0.,0.));
#26671=CARTESIAN_POINT('Origin',(-41.3,0.,0.));
#26672=CARTESIAN_POINT('Origin',(-41.3,0.,0.));
#26673=CARTESIAN_POINT('Origin',(-41.3,0.,0.));
#26674=CARTESIAN_POINT('Origin',(-41.3,0.,0.));
#26675=CARTESIAN_POINT('',(-41.3,-1.3,10.519980988576));
#26676=CARTESIAN_POINT('Origin',(-41.3,0.,0.));
#26677=CARTESIAN_POINT('',(-41.3,-1.3,5.65));
#26678=CARTESIAN_POINT('Origin',(-27.3,0.,0.));
#26679=CARTESIAN_POINT('Origin',(75.,-3.,12.5));
#26680=CARTESIAN_POINT('',(75.,-3.,12.1346610995116));
#26681=CARTESIAN_POINT('',(75.,3.,12.1346610995116));
#26682=CARTESIAN_POINT('Origin',(75.,0.,0.));
#26683=CARTESIAN_POINT('',(75.,-3.,9.));
#26684=CARTESIAN_POINT('',(75.,-3.,12.5));
#26685=CARTESIAN_POINT('',(75.,3.,9.));
#26686=CARTESIAN_POINT('',(75.,3.,9.));
#26687=CARTESIAN_POINT('',(75.,3.,12.5));
#26688=CARTESIAN_POINT('Origin',(75.,3.,12.5));
#26689=CARTESIAN_POINT('',(115.,3.,12.1346610995116));
#26690=CARTESIAN_POINT('',(109.05,3.,12.1346610995116));
#26691=CARTESIAN_POINT('',(115.,3.,9.));
#26692=CARTESIAN_POINT('',(115.,3.,9.));
#26693=CARTESIAN_POINT('',(115.,3.,12.5));
#26694=CARTESIAN_POINT('Origin',(115.,-3.,12.5));
#26695=CARTESIAN_POINT('',(115.,-3.,12.1346610995116));
#26696=CARTESIAN_POINT('',(109.05,-3.,12.1346610995116));
#26697=CARTESIAN_POINT('',(115.,-3.,9.));
#26698=CARTESIAN_POINT('',(115.,-3.,12.5));
#26699=CARTESIAN_POINT('',(75.,-3.,9.));
#26700=CARTESIAN_POINT('Origin',(115.,3.,12.5));
#26701=CARTESIAN_POINT('Origin',(115.,0.,0.));
#26702=CARTESIAN_POINT('',(115.,-3.,9.));
#26703=CARTESIAN_POINT('Origin',(95.,0.,9.));
#26704=CARTESIAN_POINT('Origin',(-41.3,4.10027901074542,10.6097932135382));
#26705=CARTESIAN_POINT('Origin',(-40.8,0.,0.));
#26706=CARTESIAN_POINT('Origin',(-40.8,0.,0.));
#26707=CARTESIAN_POINT('Origin',(-40.8,0.,0.));
#26708=CARTESIAN_POINT('Origin',(-40.8,0.,0.));
#26709=CARTESIAN_POINT('Origin',(-16.3,2.50084869180498,-10.1463419921022));
#26710=CARTESIAN_POINT('Origin',(-40.8,0.,0.));
#26711=CARTESIAN_POINT('Origin',(-40.8,0.,0.));
#26712=CARTESIAN_POINT('Origin',(-40.8,0.,0.));
#26713=CARTESIAN_POINT('Origin',(-40.8,0.,0.));
#26714=CARTESIAN_POINT('Origin',(-40.8,0.,0.));
#26715=CARTESIAN_POINT('Origin',(-41.3,-1.3,11.3));
#26716=CARTESIAN_POINT('Ctrl Pts',(-41.2927947172303,-1.3,10.5236110236165));
#26717=CARTESIAN_POINT('Ctrl Pts',(-41.2963979800735,-1.3,10.521795697712));
#26718=CARTESIAN_POINT('Ctrl Pts',(-41.3,-1.3,10.519980988576));
#26719=CARTESIAN_POINT('Origin',(-40.8,0.,0.));
#26720=CARTESIAN_POINT('Origin',(-9.5,15.,0.));
#26721=CARTESIAN_POINT('',(-9.49999999999999,-15.,-1.83697019872103E-15));
#26722=CARTESIAN_POINT('Origin',(-9.49999999999999,0.,0.));
#26723=CARTESIAN_POINT('Origin',(2.25,0.,0.));
#26724=CARTESIAN_POINT('',(14.,-15.,-1.83697019872103E-15));
#26725=CARTESIAN_POINT('Origin',(14.,0.,0.));
#26726=CARTESIAN_POINT('',(2.25,-15.,-1.83697019872103E-15));
#26727=CARTESIAN_POINT('Origin',(14.,14.,0.));
#26728=CARTESIAN_POINT('',(14.,-14.,-1.71450551880629E-15));
#26729=CARTESIAN_POINT('Origin',(14.,0.,0.));
#26730=CARTESIAN_POINT('Origin',(39.9,0.,0.));
#26731=CARTESIAN_POINT('',(65.8,-14.,-1.71450551880629E-15));
#26732=CARTESIAN_POINT('Origin',(65.8,0.,0.));
#26733=CARTESIAN_POINT('',(39.9,-14.,-1.71450551880629E-15));
#26734=CARTESIAN_POINT('Origin',(65.8,12.5,0.));
#26735=CARTESIAN_POINT('',(65.8,-12.5,-1.53080849893419E-15));
#26736=CARTESIAN_POINT('Origin',(65.8,0.,0.));
#26737=CARTESIAN_POINT('Origin',(109.05,0.,0.));
#26738=CARTESIAN_POINT('',(152.3,-12.5,-1.53080849893419E-15));
#26739=CARTESIAN_POINT('Origin',(152.3,0.,0.));
#26740=CARTESIAN_POINT('',(109.05,-12.5,-1.53080849893419E-15));
#26741=CARTESIAN_POINT('Origin',(152.55,0.,0.));
#26742=CARTESIAN_POINT('',(152.8,-12.,-1.46957615897682E-15));
#26743=CARTESIAN_POINT('Origin',(152.8,0.,0.));
#26744=CARTESIAN_POINT('',(152.55,-12.25,-1.50019232895551E-15));
#26745=CARTESIAN_POINT('Origin',(152.8,0.,0.));
#26746=CARTESIAN_POINT('',(0.,0.,0.));
#26747=CARTESIAN_POINT('Origin',(75.17,-1.495,9.13));
#26748=CARTESIAN_POINT('',(75.14,2.84,9.16));
#26749=CARTESIAN_POINT('',(75.29,2.69,9.01));
#26750=CARTESIAN_POINT('',(75.8575,2.1225,8.4425));
#26751=CARTESIAN_POINT('',(75.29,-2.69,9.01));
#26752=CARTESIAN_POINT('',(75.29,-1.495,9.01));
#26753=CARTESIAN_POINT('',(75.14,-2.84,9.16));
#26754=CARTESIAN_POINT('',(75.3591666666667,-2.62083333333333,8.94083333333333));
#26755=CARTESIAN_POINT('',(75.05,-2.75,9.25));
#26756=CARTESIAN_POINT('',(74.2120833333333,-1.91208333333334,10.0879166666667));
#26757=CARTESIAN_POINT('',(75.05,2.75,9.25));
#26758=CARTESIAN_POINT('',(75.05,-1.495,9.25));
#26759=CARTESIAN_POINT('',(74.2129166666667,1.91291666666666,10.0870833333333));
#26760=CARTESIAN_POINT('Origin',(75.05,-2.99,9.01));
#26761=CARTESIAN_POINT('',(114.71,2.69,9.01));
#26762=CARTESIAN_POINT('',(75.05,2.69,9.01));
#26763=CARTESIAN_POINT('',(114.71,-2.69,9.01));
#26764=CARTESIAN_POINT('',(114.71,-1.495,9.01));
#26765=CARTESIAN_POINT('',(75.05,-2.69,9.01));
#26766=CARTESIAN_POINT('Origin',(75.05,2.84,9.16));
#26767=CARTESIAN_POINT('',(75.29,2.99,9.31));
#26768=CARTESIAN_POINT('',(75.3595833333333,3.05958333333333,9.37958333333333));
#26769=CARTESIAN_POINT('',(114.71,2.99,9.31));
#26770=CARTESIAN_POINT('',(75.05,2.99,9.31));
#26771=CARTESIAN_POINT('',(114.86,2.84,9.16));
#26772=CARTESIAN_POINT('',(107.990416666667,9.70958333333326,16.0295833333333));
#26773=CARTESIAN_POINT('',(107.4925,-4.52749999999994,1.79250000000006));
#26774=CARTESIAN_POINT('Origin',(75.17,2.87,10.5075));
#26775=CARTESIAN_POINT('',(75.05,2.75,14.76));
#26776=CARTESIAN_POINT('',(75.05,2.75,10.5075));
#26777=CARTESIAN_POINT('',(75.14,2.84,14.85));
#26778=CARTESIAN_POINT('',(74.2120833333333,1.91208333333334,13.9220833333333));
#26779=CARTESIAN_POINT('',(75.29,2.99,14.7));
#26780=CARTESIAN_POINT('',(75.85875,3.55875,14.13125));
#26781=CARTESIAN_POINT('',(75.29,2.99,10.5075));
#26782=CARTESIAN_POINT('Origin',(75.17,1.495,14.88));
#26783=CARTESIAN_POINT('',(75.14,-2.84,14.85));
#26784=CARTESIAN_POINT('',(75.29,-2.69,15.));
#26785=CARTESIAN_POINT('',(75.8575,-2.12250000000001,15.5675));
#26786=CARTESIAN_POINT('',(75.29,2.69,15.));
#26787=CARTESIAN_POINT('',(75.29,1.495,15.));
#26788=CARTESIAN_POINT('',(75.3591666666667,2.62083333333333,15.0691666666667));
#26789=CARTESIAN_POINT('',(75.05,-2.75,14.76));
#26790=CARTESIAN_POINT('',(75.05,1.495,14.76));
#26791=CARTESIAN_POINT('',(74.2129166666667,-1.91291666666667,13.9229166666667));
#26792=CARTESIAN_POINT('Origin',(75.05,2.99,15.));
#26793=CARTESIAN_POINT('',(114.71,-2.69,15.));
#26794=CARTESIAN_POINT('',(75.05,-2.69,15.));
#26795=CARTESIAN_POINT('',(114.71,2.69,15.));
#26796=CARTESIAN_POINT('',(114.71,1.495,15.));
#26797=CARTESIAN_POINT('',(75.05,2.69,15.));
#26798=CARTESIAN_POINT('Origin',(75.05,-2.84,14.85));
#26799=CARTESIAN_POINT('',(75.29,-2.99,14.7));
#26800=CARTESIAN_POINT('',(75.3595833333333,-3.05958333333334,14.6304166666667));
#26801=CARTESIAN_POINT('',(114.71,-2.99,14.7));
#26802=CARTESIAN_POINT('',(75.05,-2.99,14.7));
#26803=CARTESIAN_POINT('',(114.86,-2.84,14.85));
#26804=CARTESIAN_POINT('',(107.990416666667,-9.70958333333323,7.98041666666672));
#26805=CARTESIAN_POINT('',(107.4925,4.52749999999992,22.2175));
#26806=CARTESIAN_POINT('Origin',(75.17,-2.87,13.5025));
#26807=CARTESIAN_POINT('',(75.29,-2.99,9.31));
#26808=CARTESIAN_POINT('',(75.85875,-3.55875,9.87875));
#26809=CARTESIAN_POINT('',(75.29,-2.99,13.5025));
#26810=CARTESIAN_POINT('',(75.05,-2.75,13.5025));
#26811=CARTESIAN_POINT('Origin',(75.05,2.99,9.01));
#26812=CARTESIAN_POINT('',(114.71,2.99,14.7));
#26813=CARTESIAN_POINT('',(75.05,2.99,14.7));
#26814=CARTESIAN_POINT('',(114.71,2.99,10.5075));
#26815=CARTESIAN_POINT('Origin',(114.83,1.495,14.88));
#26816=CARTESIAN_POINT('',(114.95,-2.75,14.76));
#26817=CARTESIAN_POINT('',(115.787083333333,-1.91291666666665,13.9229166666666));
#26818=CARTESIAN_POINT('',(114.95,2.75,14.76));
#26819=CARTESIAN_POINT('',(114.95,1.495,14.76));
#26820=CARTESIAN_POINT('',(114.86,2.84,14.85));
#26821=CARTESIAN_POINT('',(115.787916666667,1.91208333333331,13.9220833333333));
#26822=CARTESIAN_POINT('',(107.990833333334,-4.02916666666659,21.7191666666666));
#26823=CARTESIAN_POINT('Origin',(114.83,2.87,10.5075));
#26824=CARTESIAN_POINT('',(114.95,2.75,9.25));
#26825=CARTESIAN_POINT('',(114.95,2.75,10.5075));
#26826=CARTESIAN_POINT('',(115.787083333333,1.91291666666665,10.0870833333334));
#26827=CARTESIAN_POINT('',(107.49125,10.2087499999999,7.48125000000006));
#26828=CARTESIAN_POINT('Origin',(114.95,0.,12.005));
#26829=CARTESIAN_POINT('',(114.95,-2.75,9.25));
#26830=CARTESIAN_POINT('',(114.95,-2.75,13.5025));
#26831=CARTESIAN_POINT('',(114.95,-1.495,9.25));
#26832=CARTESIAN_POINT('Origin',(114.83,-2.87,13.5025));
#26833=CARTESIAN_POINT('',(114.71,-2.99,9.31));
#26834=CARTESIAN_POINT('',(114.71,-2.99,13.5025));
#26835=CARTESIAN_POINT('',(114.86,-2.84,9.16000000000001));
#26836=CARTESIAN_POINT('',(107.49125,-10.2087499999999,16.5287499999999));
#26837=CARTESIAN_POINT('',(115.787916666667,-1.91208333333331,10.0879166666667));
#26838=CARTESIAN_POINT('Origin',(114.83,-1.495,9.13));
#26839=CARTESIAN_POINT('',(107.990833333334,4.02916666666659,2.29083333333341));
#26840=CARTESIAN_POINT('Origin',(75.05,-2.84,9.16));
#26841=CARTESIAN_POINT('',(75.05,-2.99,9.31));
#26842=CARTESIAN_POINT('Origin',(75.05,-2.99,15.));
#26843=CARTESIAN_POINT('Origin',(75.05,2.84,14.85));
#26844=CARTESIAN_POINT('Origin',(75.05,0.,12.005));
#26845=CARTESIAN_POINT('',(0.,0.,0.));
#26846=CARTESIAN_POINT('Origin',(0.35,0.,0.));
#26847=CARTESIAN_POINT('',(0.7,-19.3,-2.36356832235439E-15));
#26848=CARTESIAN_POINT('Origin',(0.7,0.,0.));
#26849=CARTESIAN_POINT('',(-4.85722573273506E-16,-19.,-2.32682891837997E-15));
#26850=CARTESIAN_POINT('',(0.35,-19.15,-2.34519862036718E-15));
#26851=CARTESIAN_POINT('Origin',(0.,0.,0.));
#26852=CARTESIAN_POINT('Origin',(0.7,23.8,0.));
#26853=CARTESIAN_POINT('',(0.7,-23.8,-2.9146593819707E-15));
#26854=CARTESIAN_POINT('Origin',(0.7,0.,0.));
#26855=CARTESIAN_POINT('Origin',(0.35,0.,0.));
#26856=CARTESIAN_POINT('',(-1.04083408558608E-15,-24.,-2.93915231795365E-15));
#26857=CARTESIAN_POINT('',(0.35,-23.9,-2.92690584996217E-15));
#26858=CARTESIAN_POINT('Origin',(0.,0.,0.));
#26859=CARTESIAN_POINT('Origin',(0.,27.1,0.));
#26860=CARTESIAN_POINT('',(-4.85722573273506E-16,-27.1,-3.31879282568933E-15));
#26861=CARTESIAN_POINT('Origin',(0.,0.,0.));
#26862=CARTESIAN_POINT('Origin',(0.2,0.,0.));
#26863=CARTESIAN_POINT('',(0.4,-27.5,-3.36777869765522E-15));
#26864=CARTESIAN_POINT('Origin',(0.4,0.,0.));
#26865=CARTESIAN_POINT('',(0.2,-27.3,-3.34328576167227E-15));
#26866=CARTESIAN_POINT('Origin',(6.5,0.,0.));
#26867=CARTESIAN_POINT('',(12.6,-27.5,-3.36777869765522E-15));
#26868=CARTESIAN_POINT('Origin',(12.6,0.,0.));
#26869=CARTESIAN_POINT('',(6.5,-27.5,-3.36777869765522E-15));
#26870=CARTESIAN_POINT('Origin',(12.8,0.,0.));
#26871=CARTESIAN_POINT('',(13.,-27.1,-3.31879282568933E-15));
#26872=CARTESIAN_POINT('Origin',(13.,0.,0.));
#26873=CARTESIAN_POINT('',(12.8,-27.3,-3.34328576167227E-15));
#26874=CARTESIAN_POINT('Origin',(13.,24.,0.));
#26875=CARTESIAN_POINT('',(13.,-24.,-2.93915231795365E-15));
#26876=CARTESIAN_POINT('Origin',(13.,0.,0.));
#26877=CARTESIAN_POINT('Origin',(12.65,0.,0.));
#26878=CARTESIAN_POINT('',(12.3,-23.8,-2.9146593819707E-15));
#26879=CARTESIAN_POINT('',(12.65,-23.9,-2.92690584996217E-15));
#26880=CARTESIAN_POINT('Origin',(12.3,0.,0.));
#26881=CARTESIAN_POINT('Origin',(12.3,19.3,0.));
#26882=CARTESIAN_POINT('',(12.3,-19.3,-2.36356832235439E-15));
#26883=CARTESIAN_POINT('Origin',(12.3,0.,0.));
#26884=CARTESIAN_POINT('Origin',(12.65,0.,0.));
#26885=CARTESIAN_POINT('',(13.,-19.,-2.32682891837997E-15));
#26886=CARTESIAN_POINT('Origin',(13.,0.,0.));
#26887=CARTESIAN_POINT('',(12.65,-19.15,-2.34519862036718E-15));
#26888=CARTESIAN_POINT('Origin',(13.,15.4,0.));
#26889=CARTESIAN_POINT('',(13.,-15.4,-1.88595607068692E-15));
#26890=CARTESIAN_POINT('Origin',(13.,0.,0.));
#26891=CARTESIAN_POINT('Origin',(12.8,0.,0.));
#26892=CARTESIAN_POINT('',(12.6,-15.,-1.83697019872103E-15));
#26893=CARTESIAN_POINT('',(12.8,-15.2,-1.86146313470398E-15));
#26894=CARTESIAN_POINT('Origin',(12.6,0.,0.));
#26895=CARTESIAN_POINT('Origin',(6.5,0.,0.));
#26896=CARTESIAN_POINT('',(0.4,-15.,-1.83697019872103E-15));
#26897=CARTESIAN_POINT('',(6.5,-15.,-1.83697019872103E-15));
#26898=CARTESIAN_POINT('Origin',(0.4,0.,0.));
#26899=CARTESIAN_POINT('Origin',(0.2,0.,0.));
#26900=CARTESIAN_POINT('',(-2.42861286636753E-16,-15.4,-1.88595607068692E-15));
#26901=CARTESIAN_POINT('',(0.2,-15.2,-1.86146313470398E-15));
#26902=CARTESIAN_POINT('Origin',(0.,0.,0.));
#26903=CARTESIAN_POINT('Origin',(0.,19.,0.));
#26904=CARTESIAN_POINT('',(0.,0.,0.));
#26905=CARTESIAN_POINT('Origin',(10.,0.,0.));
#26906=CARTESIAN_POINT('',(18.8,-12.5,-1.53080849893419E-15));
#26907=CARTESIAN_POINT('Origin',(18.8,0.,0.));
#26908=CARTESIAN_POINT('',(1.2,-12.5,-1.53080849893419E-15));
#26909=CARTESIAN_POINT('',(10.,-12.5,-1.53080849893419E-15));
#26910=CARTESIAN_POINT('Origin',(1.2,0.,0.));
#26911=CARTESIAN_POINT('Origin',(1.2,15.6,0.));
#26912=CARTESIAN_POINT('',(1.2,-15.6,-1.91044900666987E-15));
#26913=CARTESIAN_POINT('Origin',(1.2,0.,0.));
#26914=CARTESIAN_POINT('Origin',(18.8,12.5,0.));
#26915=CARTESIAN_POINT('',(18.8,-15.6,-1.91044900666987E-15));
#26916=CARTESIAN_POINT('Origin',(18.8,0.,0.));
#26917=CARTESIAN_POINT('Origin',(10.,0.,0.));
#26918=CARTESIAN_POINT('',(19.3,-15.6,-1.91044900666987E-15));
#26919=CARTESIAN_POINT('Origin',(19.3,0.,0.));
#26920=CARTESIAN_POINT('',(10.,-15.6,-1.91044900666987E-15));
#26921=CARTESIAN_POINT('Origin',(0.35,0.,0.));
#26922=CARTESIAN_POINT('',(0.7,-13.5,-1.65327317884893E-15));
#26923=CARTESIAN_POINT('Origin',(0.7,0.,0.));
#26924=CARTESIAN_POINT('',(0.,-13.5,-1.65327317884893E-15));
#26925=CARTESIAN_POINT('',(0.35,-13.5,-1.65327317884893E-15));
#26926=CARTESIAN_POINT('Origin',(0.,0.,0.));
#26927=CARTESIAN_POINT('Origin',(0.,16.5,0.));
#26928=CARTESIAN_POINT('',(0.,-16.5,-2.02066721859313E-15));
#26929=CARTESIAN_POINT('Origin',(0.,0.,0.));
#26930=CARTESIAN_POINT('Origin',(10.,0.,0.));
#26931=CARTESIAN_POINT('',(20.,-16.5,-2.02066721859313E-15));
#26932=CARTESIAN_POINT('Origin',(20.,0.,0.));
#26933=CARTESIAN_POINT('',(10.,-16.5,-2.02066721859313E-15));
#26934=CARTESIAN_POINT('Origin',(20.,13.5,0.));
#26935=CARTESIAN_POINT('',(20.,-13.5,-1.65327317884893E-15));
#26936=CARTESIAN_POINT('Origin',(20.,0.,0.));
#26937=CARTESIAN_POINT('Origin',(19.65,0.,0.));
#26938=CARTESIAN_POINT('',(19.3,-13.5,-1.65327317884893E-15));
#26939=CARTESIAN_POINT('',(19.65,-13.5,-1.65327317884893E-15));
#26940=CARTESIAN_POINT('Origin',(19.3,0.,0.));
#26941=CARTESIAN_POINT('Origin',(19.3,15.6,0.));
#26942=CARTESIAN_POINT('Origin',(10.,0.,0.));
#26943=CARTESIAN_POINT('',(0.7,-15.6,-1.91044900666987E-15));
#26944=CARTESIAN_POINT('',(10.,-15.6,-1.91044900666987E-15));
#26945=CARTESIAN_POINT('Origin',(0.7,0.,0.));
#26946=CARTESIAN_POINT('Origin',(0.7,13.5,0.));
#26947=CARTESIAN_POINT('',(0.,0.,0.));
#26948=CARTESIAN_POINT('Origin',(6.86,0.,0.));
#26949=CARTESIAN_POINT('',(6.72,20.5,-2.51052593825207E-15));
#26950=CARTESIAN_POINT('',(6.72,-20.5,-2.51052593825207E-15));
#26951=CARTESIAN_POINT('Origin',(6.72,0.,0.));
#26952=CARTESIAN_POINT('Origin',(6.72,0.,0.));
#26953=CARTESIAN_POINT('',(7.,20.78,2.5448160486282E-15));
#26954=CARTESIAN_POINT('',(6.86,20.64,-2.52767099344014E-15));
#26955=CARTESIAN_POINT('Origin',(7.,0.,0.));
#26956=CARTESIAN_POINT('Origin',(7.,20.5,0.));
#26957=CARTESIAN_POINT('',(7.,-23.52,-2.88036927159457E-15));
#26958=CARTESIAN_POINT('Origin',(7.,0.,0.));
#26959=CARTESIAN_POINT('Origin',(6.25,0.,0.));
#26960=CARTESIAN_POINT('',(5.5,-20.5,-2.51052593825207E-15));
#26961=CARTESIAN_POINT('',(6.25,-20.5,-2.51052593825207E-15));
#26962=CARTESIAN_POINT('Origin',(5.5,0.,0.));
#26963=CARTESIAN_POINT('Origin',(0.0776580274715325,0.,-5.27607663745458E-16));
#26964=CARTESIAN_POINT('',(0.155316054943065,17.2329740824146,-2.11043065498183E-15));
#26965=CARTESIAN_POINT('',(0.155316054943064,-17.2329740824146,-2.11043065498183E-15));
#26966=CARTESIAN_POINT('Origin',(0.155316054943065,0.,-1.05521532749092E-15));
#26967=CARTESIAN_POINT('Origin',(0.155316054943065,0.,-1.05521532749092E-15));
#26968=CARTESIAN_POINT('',(0.,16.72,2.04760944817437E-15));
#26969=CARTESIAN_POINT('',(0.0776580274715325,16.9764870412073,2.0790200515781E-15));
#26970=CARTESIAN_POINT('Origin',(0.,0.,0.));
#26971=CARTESIAN_POINT('Origin',(0.,17.,0.));
#26972=CARTESIAN_POINT('',(0.,-15.,-1.83697019872103E-15));
#26973=CARTESIAN_POINT('Origin',(0.,0.,0.));
#26974=CARTESIAN_POINT('Origin',(0.5,0.,0.));
#26975=CARTESIAN_POINT('',(1.,-18.5,-2.2655965784226E-15));
#26976=CARTESIAN_POINT('Origin',(1.,0.,0.));
#26977=CARTESIAN_POINT('',(0.5,-17.75,-2.17374806848655E-15));
#26978=CARTESIAN_POINT('Origin',(1.75,0.,0.));
#26979=CARTESIAN_POINT('',(3.5,-15.,-1.83697019872103E-15));
#26980=CARTESIAN_POINT('Origin',(3.5,0.,0.));
#26981=CARTESIAN_POINT('',(1.75,-15.,-1.83697019872103E-15));
#26982=CARTESIAN_POINT('Origin',(1.,23.52,0.));
#26983=CARTESIAN_POINT('',(1.,-23.52,-2.88036927159457E-15));
#26984=CARTESIAN_POINT('Origin',(1.,0.,0.));
#26985=CARTESIAN_POINT('Origin',(4.,0.,0.));
#26986=CARTESIAN_POINT('',(4.,-23.52,-2.88036927159457E-15));
#26987=CARTESIAN_POINT('Origin',(5.5,18.,0.));
#26988=CARTESIAN_POINT('',(5.5,-18.,-2.20436423846524E-15));
#26989=CARTESIAN_POINT('Origin',(5.5,0.,0.));
#26990=CARTESIAN_POINT('Origin',(4.5,0.,0.));
#26991=CARTESIAN_POINT('',(4.5,-16.5,-2.02066721859313E-15));
#26992=CARTESIAN_POINT('',(0.,0.,0.));
#26993=CARTESIAN_POINT('Origin',(59.75,0.,0.));
#26994=CARTESIAN_POINT('',(60.,-4.5,-5.51091059616309E-16));
#26995=CARTESIAN_POINT('Origin',(60.,0.,0.));
#26996=CARTESIAN_POINT('',(59.5,-4.,4.89858719658941E-16));
#26997=CARTESIAN_POINT('',(59.75,-4.25,-5.20474889637625E-16));
#26998=CARTESIAN_POINT('Origin',(59.5,0.,0.));
#26999=CARTESIAN_POINT('Origin',(50.05,0.,0.));
#27000=CARTESIAN_POINT('',(40.,-4.,-4.89858719658941E-16));
#27001=CARTESIAN_POINT('Origin',(40.,0.,0.));
#27002=CARTESIAN_POINT('',(50.05,-4.,-4.89858719658941E-16));
#27003=CARTESIAN_POINT('Origin',(60.,0.,0.));
#27004=CARTESIAN_POINT('',(60.,-8.,-9.79717439317882E-16));
#27005=CARTESIAN_POINT('Origin',(60.,0.,0.));
#27006=CARTESIAN_POINT('Origin',(26.5,0.,0.));
#27007=CARTESIAN_POINT('',(-6.92828513265203,-1.,-1.22464679914735E-16));
#27008=CARTESIAN_POINT('',(-6.92828513265203,-1.22464679914735E-16,1.));
#27009=CARTESIAN_POINT('Origin',(-6.92828513265203,0.,0.));
#27010=CARTESIAN_POINT('',(40.,-1.,1.22464679914735E-16));
#27011=CARTESIAN_POINT('',(26.5,-1.,-1.22464679914735E-16));
#27012=CARTESIAN_POINT('Origin',(40.,0.,0.));
#27013=CARTESIAN_POINT('Origin',(-6.92828513265203,0.,0.));
#27014=CARTESIAN_POINT('Origin',(40.,4.,0.));
#27015=CARTESIAN_POINT('Origin',(12.872281323269,0.,0.));
#27016=CARTESIAN_POINT('',(20.,-4.,-4.89858719658941E-16));
#27017=CARTESIAN_POINT('Origin',(20.,0.,0.));
#27018=CARTESIAN_POINT('',(5.74456264653803,-4.,-4.89858719658941E-16));
#27019=CARTESIAN_POINT('',(12.872281323269,-4.,-4.89858719658941E-16));
#27020=CARTESIAN_POINT('',(5.74456264653803,-4.89858719658941E-16,4.));
#27021=CARTESIAN_POINT('Origin',(5.74456264653803,0.,0.));
#27022=CARTESIAN_POINT('Origin',(5.74456264653803,0.,0.));
#27023=CARTESIAN_POINT('Origin',(20.,8.,0.));
#27024=CARTESIAN_POINT('',(20.,-8.,-9.79717439317883E-16));
#27025=CARTESIAN_POINT('Origin',(20.,0.,0.));
#27026=CARTESIAN_POINT('Origin',(20.25,0.,0.));
#27027=CARTESIAN_POINT('',(20.5,-8.5,-1.04094977927525E-15));
#27028=CARTESIAN_POINT('Origin',(20.5,0.,0.));
#27029=CARTESIAN_POINT('',(20.25,-8.25,-1.01033360929657E-15));
#27030=CARTESIAN_POINT('Origin',(40.,0.,0.));
#27031=CARTESIAN_POINT('',(59.5,-8.5,-1.04094977927525E-15));
#27032=CARTESIAN_POINT('Origin',(59.5,0.,0.));
#27033=CARTESIAN_POINT('',(40.,-8.5,-1.04094977927525E-15));
#27034=CARTESIAN_POINT('Origin',(59.75,0.,0.));
#27035=CARTESIAN_POINT('',(59.75,-8.25,-1.01033360929657E-15));
#27036=CARTESIAN_POINT('Ctrl Pts',(-6.92828513265203,0.,1.));
#27037=CARTESIAN_POINT('Ctrl Pts',(-6.92828513265203,-1.,1.));
#27038=CARTESIAN_POINT('Ctrl Pts',(-6.92828513265203,-1.,0.));
#27039=CARTESIAN_POINT('Ctrl Pts',(-6.92828513265203,-1.,-1.));
#27040=CARTESIAN_POINT('Ctrl Pts',(-6.92828513265203,0.,-1.));
#27041=CARTESIAN_POINT('Ctrl Pts',(-6.92828513265203,1.,-1.));
#27042=CARTESIAN_POINT('Ctrl Pts',(-6.92828513265203,1.,0.));
#27043=CARTESIAN_POINT('Ctrl Pts',(-6.92828513265203,1.,1.));
#27044=CARTESIAN_POINT('Ctrl Pts',(-6.92828513265203,0.,1.));
#27045=CARTESIAN_POINT('Ctrl Pts',(-6.24814779917882,0.,5.71479842490333));
#27046=CARTESIAN_POINT('Ctrl Pts',(-6.24814779917882,-5.71479842490333,
5.71479842490333));
#27047=CARTESIAN_POINT('Ctrl Pts',(-6.24814779917882,-5.71479842490333,
0.));
#27048=CARTESIAN_POINT('Ctrl Pts',(-6.24814779917882,-5.71479842490333,
-5.71479842490333));
#27049=CARTESIAN_POINT('Ctrl Pts',(-6.24814779917882,0.,-5.71479842490333));
#27050=CARTESIAN_POINT('Ctrl Pts',(-6.24814779917882,5.71479842490333,-5.71479842490333));
#27051=CARTESIAN_POINT('Ctrl Pts',(-6.24814779917882,5.71479842490333,0.));
#27052=CARTESIAN_POINT('Ctrl Pts',(-6.24814779917882,5.71479842490333,5.71479842490333));
#27053=CARTESIAN_POINT('Ctrl Pts',(-6.24814779917882,0.,5.71479842490333));
#27054=CARTESIAN_POINT('Ctrl Pts',(-1.61265982287702,0.,6.81214167175753));
#27055=CARTESIAN_POINT('Ctrl Pts',(-1.61265982287702,-6.81214167175752,
6.81214167175752));
#27056=CARTESIAN_POINT('Ctrl Pts',(-1.61265982287702,-6.81214167175753,
0.));
#27057=CARTESIAN_POINT('Ctrl Pts',(-1.61265982287702,-6.81214167175752,
-6.81214167175752));
#27058=CARTESIAN_POINT('Ctrl Pts',(-1.61265982287702,0.,-6.81214167175753));
#27059=CARTESIAN_POINT('Ctrl Pts',(-1.61265982287702,6.81214167175752,-6.81214167175752));
#27060=CARTESIAN_POINT('Ctrl Pts',(-1.61265982287702,6.81214167175753,0.));
#27061=CARTESIAN_POINT('Ctrl Pts',(-1.61265982287702,6.81214167175752,6.81214167175752));
#27062=CARTESIAN_POINT('Ctrl Pts',(-1.61265982287702,0.,6.81214167175753));
#27063=CARTESIAN_POINT('Ctrl Pts',(3.02282815342477,0.,7.90948491861172));
#27064=CARTESIAN_POINT('Ctrl Pts',(3.02282815342477,-7.90948491861172,7.90948491861172));
#27065=CARTESIAN_POINT('Ctrl Pts',(3.02282815342477,-7.90948491861172,0.));
#27066=CARTESIAN_POINT('Ctrl Pts',(3.02282815342477,-7.90948491861172,-7.90948491861172));
#27067=CARTESIAN_POINT('Ctrl Pts',(3.02282815342477,0.,-7.90948491861172));
#27068=CARTESIAN_POINT('Ctrl Pts',(3.02282815342477,7.90948491861172,-7.90948491861172));
#27069=CARTESIAN_POINT('Ctrl Pts',(3.02282815342477,7.90948491861172,0.));
#27070=CARTESIAN_POINT('Ctrl Pts',(3.02282815342477,7.90948491861172,7.90948491861172));
#27071=CARTESIAN_POINT('Ctrl Pts',(3.02282815342477,0.,7.90948491861172));
#27072=CARTESIAN_POINT('Ctrl Pts',(5.74456264653803,0.,4.));
#27073=CARTESIAN_POINT('Ctrl Pts',(5.74456264653803,-4.,4.));
#27074=CARTESIAN_POINT('Ctrl Pts',(5.74456264653803,-4.,0.));
#27075=CARTESIAN_POINT('Ctrl Pts',(5.74456264653803,-4.,-4.));
#27076=CARTESIAN_POINT('Ctrl Pts',(5.74456264653803,0.,-4.));
#27077=CARTESIAN_POINT('Ctrl Pts',(5.74456264653803,4.,-4.));
#27078=CARTESIAN_POINT('Ctrl Pts',(5.74456264653803,4.,0.));
#27079=CARTESIAN_POINT('Ctrl Pts',(5.74456264653803,4.,4.));
#27080=CARTESIAN_POINT('Ctrl Pts',(5.74456264653803,0.,4.));
#27081=CARTESIAN_POINT('Origin',(-0.000182197201354928,-7.10914706616621E-20,
0.000580505911673135));
#27082=CARTESIAN_POINT('',(0.,0.,0.));
#27083=CARTESIAN_POINT('Origin',(0.3,0.,0.));
#27084=CARTESIAN_POINT('',(0.6,-5.,-6.12323399573677E-16));
#27085=CARTESIAN_POINT('Origin',(0.6,0.,0.));
#27086=CARTESIAN_POINT('',(0.,-5.,-6.12323399573677E-16));
#27087=CARTESIAN_POINT('',(0.3,-5.,-6.12323399573677E-16));
#27088=CARTESIAN_POINT('Origin',(0.,0.,0.));
#27089=CARTESIAN_POINT('Origin',(0.,10.5,0.));
#27090=CARTESIAN_POINT('',(-7.97972798949331E-16,-10.5,-1.28587913910472E-15));
#27091=CARTESIAN_POINT('Origin',(0.,0.,0.));
#27092=CARTESIAN_POINT('Origin',(0.25,0.,0.));
#27093=CARTESIAN_POINT('',(0.5,-11.,-1.34711147906209E-15));
#27094=CARTESIAN_POINT('Origin',(0.5,0.,0.));
#27095=CARTESIAN_POINT('',(0.25,-10.75,-1.3164953090834E-15));
#27096=CARTESIAN_POINT('Origin',(2.25,0.,0.));
#27097=CARTESIAN_POINT('',(4.,-11.,-1.34711147906209E-15));
#27098=CARTESIAN_POINT('Origin',(4.,0.,0.));
#27099=CARTESIAN_POINT('',(2.25,-11.,-1.34711147906209E-15));
#27100=CARTESIAN_POINT('Origin',(4.,9.,0.));
#27101=CARTESIAN_POINT('',(4.,-9.,-1.10218211923262E-15));
#27102=CARTESIAN_POINT('Origin',(4.,0.,0.));
#27103=CARTESIAN_POINT('Origin',(8.75,0.,0.));
#27104=CARTESIAN_POINT('',(13.5,-9.,-1.10218211923262E-15));
#27105=CARTESIAN_POINT('Origin',(13.5,0.,0.));
#27106=CARTESIAN_POINT('',(8.75,-9.,-1.10218211923262E-15));
#27107=CARTESIAN_POINT('Origin',(13.5,6.08526088183572,0.));
#27108=CARTESIAN_POINT('',(13.5,6.08526088183572,0.));
#27109=CARTESIAN_POINT('Origin',(13.5,0.,0.));
#27110=CARTESIAN_POINT('Origin',(10.,-1.11022302462516E-15,0.));
#27111=CARTESIAN_POINT('',(3.27092874164644,-1.93429658240287E-15,-2.));
#27112=CARTESIAN_POINT('',(3.27092874164644,-1.93429658240287E-15,2.));
#27113=CARTESIAN_POINT('Origin',(3.27092874164644,0.,0.));
#27114=CARTESIAN_POINT('',(10.,-1.11022302462516E-15,-7.02));
#27115=CARTESIAN_POINT('Origin',(10.,-1.11022302462516E-15,0.));
#27116=CARTESIAN_POINT('',(3.27092874164644,-2.,-2.44929359829471E-16));
#27117=CARTESIAN_POINT('Origin',(3.27092874164644,0.,0.));
#27118=CARTESIAN_POINT('Origin',(3.27092874164644,0.,0.));
#27119=CARTESIAN_POINT('',(10.,-1.11022302462516E-15,7.02));
#27120=CARTESIAN_POINT('Origin',(10.,-1.11022302462516E-15,0.));
#27121=CARTESIAN_POINT('Origin',(1.93546437082322,0.,0.));
#27122=CARTESIAN_POINT('',(0.6,-2.,-2.44929359829471E-16));
#27123=CARTESIAN_POINT('',(1.93546437082322,-2.,-2.44929359829471E-16));
#27124=CARTESIAN_POINT('Origin',(0.6,0.,0.));
#27125=CARTESIAN_POINT('Origin',(0.6,5.,0.));
#27126=CARTESIAN_POINT('',(0.,0.,0.));
#27127=CARTESIAN_POINT('Origin',(6.9,0.,0.));
#27128=CARTESIAN_POINT('',(7.,40.8,-4.9965589405212E-15));
#27129=CARTESIAN_POINT('Origin',(7.,0.,0.));
#27130=CARTESIAN_POINT('',(6.8,41.,5.02105187650415E-15));
#27131=CARTESIAN_POINT('',(6.9,40.9,5.00880540851267E-15));
#27132=CARTESIAN_POINT('',(6.8,-41.,-5.02105187650415E-15));
#27133=CARTESIAN_POINT('Origin',(6.8,0.,0.));
#27134=CARTESIAN_POINT('Origin',(6.8,0.,0.));
#27135=CARTESIAN_POINT('Origin',(7.,22.,0.));
#27136=CARTESIAN_POINT('',(7.,11.9691009237861,18.4591609526604));
#27137=CARTESIAN_POINT('',(7.,20.6597267643837,7.56146083908438));
#27138=CARTESIAN_POINT('Origin',(7.,22.4545685280471,17.9069208599539));
#27139=CARTESIAN_POINT('',(7.,21.894565536133,2.15127868579955));
#27140=CARTESIAN_POINT('Origin',(7.,0.,0.));
#27141=CARTESIAN_POINT('',(7.,18.7929170842265,-11.4379310832593));
#27142=CARTESIAN_POINT('Origin',(7.,28.0003889647509,-6.39090606159037));
#27143=CARTESIAN_POINT('',(7.,15.3329757320272,-15.7765603095562));
#27144=CARTESIAN_POINT('Origin',(7.,0.,0.));
#27145=CARTESIAN_POINT('',(7.,2.77465753400022,-21.8243276086347));
#27146=CARTESIAN_POINT('Origin',(7.,12.4613454071529,-25.8762503680314));
#27147=CARTESIAN_POINT('',(7.,-2.77465753400023,-21.8243276086347));
#27148=CARTESIAN_POINT('Origin',(7.,0.,0.));
#27149=CARTESIAN_POINT('',(7.,-15.3329757320272,-15.7765603095562));
#27150=CARTESIAN_POINT('Origin',(7.,-12.4613454071529,-25.8762503680314));
#27151=CARTESIAN_POINT('',(7.,-18.7929170842265,-11.4379310832593));
#27152=CARTESIAN_POINT('Origin',(7.,0.,0.));
#27153=CARTESIAN_POINT('',(7.,-21.894565536133,2.15127868579957));
#27154=CARTESIAN_POINT('Origin',(7.,-28.0003889647509,-6.39090606159036));
#27155=CARTESIAN_POINT('',(7.,-20.6597267643837,7.56146083908439));
#27156=CARTESIAN_POINT('Origin',(7.,0.,0.));
#27157=CARTESIAN_POINT('',(7.,-11.9691009237861,18.4591609526604));
#27158=CARTESIAN_POINT('Origin',(7.,-22.4545685280471,17.9069208599539));
#27159=CARTESIAN_POINT('',(7.,-6.96934080933589,20.8669185239059));
#27160=CARTESIAN_POINT('Origin',(7.,0.,0.));
#27161=CARTESIAN_POINT('',(7.,6.96934080933589,20.8669185239059));
#27162=CARTESIAN_POINT('Origin',(7.,0.,28.7204711393357));
#27163=CARTESIAN_POINT('Origin',(7.,0.,0.));
#27164=CARTESIAN_POINT('Origin',(5.75,0.,0.));
#27165=CARTESIAN_POINT('',(4.5,-41.,-5.02105187650415E-15));
#27166=CARTESIAN_POINT('',(5.75,-41.,-5.02105187650415E-15));
#27167=CARTESIAN_POINT('Origin',(4.5,0.,0.));
#27168=CARTESIAN_POINT('Origin',(3.9,22.4545685280471,17.9069208599539));
#27169=CARTESIAN_POINT('',(4.,20.6597267643837,7.56146083908438));
#27170=CARTESIAN_POINT('',(4.,11.9691009237861,18.4591609526604));
#27171=CARTESIAN_POINT('Origin',(4.,22.4545685280471,17.9069208599539));
#27172=CARTESIAN_POINT('',(3.9,20.6597267643837,7.56146083908438));
#27173=CARTESIAN_POINT('',(3.9,11.9691009237861,18.4591609526604));
#27174=CARTESIAN_POINT('Origin',(5.5,0.,0.));
#27175=CARTESIAN_POINT('',(4.,21.894565536133,2.15127868579955));
#27176=CARTESIAN_POINT('Origin',(4.,0.,0.));
#27177=CARTESIAN_POINT('',(3.9,21.894565536133,2.15127868579956));
#27178=CARTESIAN_POINT('Origin',(3.9,28.0003889647509,-6.39090606159037));
#27179=CARTESIAN_POINT('',(4.,18.7929170842265,-11.4379310832593));
#27180=CARTESIAN_POINT('Origin',(4.,28.0003889647509,-6.39090606159037));
#27181=CARTESIAN_POINT('',(3.9,18.7929170842265,-11.4379310832593));
#27182=CARTESIAN_POINT('Origin',(5.5,0.,0.));
#27183=CARTESIAN_POINT('',(4.,15.3329757320272,-15.7765603095562));
#27184=CARTESIAN_POINT('Origin',(4.,0.,0.));
#27185=CARTESIAN_POINT('',(3.9,15.3329757320272,-15.7765603095562));
#27186=CARTESIAN_POINT('Origin',(3.9,12.4613454071529,-25.8762503680314));
#27187=CARTESIAN_POINT('',(4.,2.77465753400022,-21.8243276086347));
#27188=CARTESIAN_POINT('Origin',(4.,12.4613454071529,-25.8762503680314));
#27189=CARTESIAN_POINT('',(3.9,2.77465753400023,-21.8243276086347));
#27190=CARTESIAN_POINT('Origin',(5.5,0.,0.));
#27191=CARTESIAN_POINT('',(4.,-2.77465753400023,-21.8243276086347));
#27192=CARTESIAN_POINT('Origin',(4.,0.,0.));
#27193=CARTESIAN_POINT('',(3.9,-2.77465753400023,-21.8243276086347));
#27194=CARTESIAN_POINT('Origin',(3.9,-12.4613454071529,-25.8762503680314));
#27195=CARTESIAN_POINT('',(4.,-15.3329757320272,-15.7765603095562));
#27196=CARTESIAN_POINT('Origin',(4.,-12.4613454071529,-25.8762503680314));
#27197=CARTESIAN_POINT('',(3.9,-15.3329757320272,-15.7765603095562));
#27198=CARTESIAN_POINT('Origin',(5.5,0.,0.));
#27199=CARTESIAN_POINT('',(4.,-18.7929170842265,-11.4379310832593));
#27200=CARTESIAN_POINT('Origin',(4.,0.,0.));
#27201=CARTESIAN_POINT('',(3.9,-18.7929170842265,-11.4379310832593));
#27202=CARTESIAN_POINT('Origin',(3.9,-28.0003889647509,-6.39090606159036));
#27203=CARTESIAN_POINT('',(4.,-21.894565536133,2.15127868579957));
#27204=CARTESIAN_POINT('Origin',(4.,-28.0003889647509,-6.39090606159036));
#27205=CARTESIAN_POINT('',(3.9,-21.894565536133,2.15127868579957));
#27206=CARTESIAN_POINT('Origin',(5.5,0.,0.));
#27207=CARTESIAN_POINT('',(4.,-20.6597267643837,7.56146083908439));
#27208=CARTESIAN_POINT('Origin',(4.,0.,0.));
#27209=CARTESIAN_POINT('',(3.9,-20.6597267643837,7.56146083908439));
#27210=CARTESIAN_POINT('Origin',(3.9,-22.4545685280471,17.9069208599539));
#27211=CARTESIAN_POINT('',(4.,-11.9691009237861,18.4591609526604));
#27212=CARTESIAN_POINT('Origin',(4.,-22.4545685280471,17.9069208599539));
#27213=CARTESIAN_POINT('',(3.9,-11.9691009237861,18.4591609526604));
#27214=CARTESIAN_POINT('Origin',(5.5,0.,0.));
#27215=CARTESIAN_POINT('',(4.,-6.96934080933589,20.8669185239059));
#27216=CARTESIAN_POINT('Origin',(4.,0.,0.));
#27217=CARTESIAN_POINT('',(3.9,-6.96934080933589,20.8669185239059));
#27218=CARTESIAN_POINT('Origin',(3.9,0.,28.7204711393357));
#27219=CARTESIAN_POINT('',(4.,6.96934080933589,20.8669185239059));
#27220=CARTESIAN_POINT('Origin',(4.,0.,28.7204711393357));
#27221=CARTESIAN_POINT('',(3.9,6.96934080933589,20.8669185239059));
#27222=CARTESIAN_POINT('Origin',(4.,40.5,0.));
#27223=CARTESIAN_POINT('',(4.,-40.5,-4.95981953654678E-15));
#27224=CARTESIAN_POINT('Origin',(4.,0.,0.));
#27225=CARTESIAN_POINT('Origin',(4.,0.,0.));
#27226=CARTESIAN_POINT('Origin',(5.5,0.,0.));
#27227=CARTESIAN_POINT('Origin',(4.25,0.,0.));
#27228=CARTESIAN_POINT('',(4.25,-40.75,-4.99043570652546E-15));
#27229=CARTESIAN_POINT('',(0.,0.,0.));
#27230=CARTESIAN_POINT('Origin',(-29.75,0.,0.));
#27231=CARTESIAN_POINT('',(-59.0198748077951,-5.9168929925076,0.000147316400840244));
#27232=CARTESIAN_POINT('',(-59.2716251922048,-5.91673468093559,9.87673099418387E-5));
#27233=CARTESIAN_POINT('',(-29.75,-5.91675,-7.2459289488551E-16));
#27234=CARTESIAN_POINT('',(-59.58325,2.58403649360107,5.32282025590616));
#27235=CARTESIAN_POINT('Ctrl Pts',(-59.0198748077951,-5.9168929925076,0.000147316400840244));
#27236=CARTESIAN_POINT('Ctrl Pts',(-59.0284715689044,-5.91708038654053,
0.182755768972575));
#27237=CARTESIAN_POINT('Ctrl Pts',(-59.0370683300138,-5.90879517539952,
0.365347221437024));
#27238=CARTESIAN_POINT('Ctrl Pts',(-59.0456650911231,-5.89191334558682,
0.547140283985201));
#27239=CARTESIAN_POINT('Ctrl Pts',(-59.0920846391508,-5.80075728113219,
1.52876018602797));
#27240=CARTESIAN_POINT('Ctrl Pts',(-59.1385041871784,-5.45895580385933,
2.48710200888682));
#27241=CARTESIAN_POINT('Ctrl Pts',(-59.184923735206,-4.90835058319102,3.3048580525707));
#27242=CARTESIAN_POINT('Ctrl Pts',(-59.2313432832336,-4.35774536252271,
4.12261409625457));
#27243=CARTESIAN_POINT('Ctrl Pts',(-59.2777628312612,-3.59833639845895,
4.79978436076348));
#27244=CARTESIAN_POINT('Ctrl Pts',(-59.3241823792888,-2.72308539444232,
5.25346025315473));
#27245=CARTESIAN_POINT('Ctrl Pts',(-59.3706019273164,-1.84783439042568,
5.70713614554599));
#27246=CARTESIAN_POINT('Ctrl Pts',(-59.4170214753441,-0.856741346456157,
5.93731766581958));
#27247=CARTESIAN_POINT('Ctrl Pts',(-59.4634410233717,0.128868647897307,
5.91585348664495));
#27248=CARTESIAN_POINT('Ctrl Pts',(-59.5033773489145,0.976822651441423,
5.8973871188441));
#27249=CARTESIAN_POINT('Ctrl Pts',(-59.5433136744572,1.8207182389207,5.69265890393189));
#27250=CARTESIAN_POINT('Ctrl Pts',(-59.58325,2.58415317085807,5.32292607787877));
#27251=CARTESIAN_POINT('',(-59.58325,-2.58391981634379,5.32271443393368));
#27252=CARTESIAN_POINT('Origin',(-59.58325,0.,0.));
#27253=CARTESIAN_POINT('Ctrl Pts',(-59.58325,-2.58391981634379,5.32271443393368));
#27254=CARTESIAN_POINT('Ctrl Pts',(-59.5368304519724,-3.47102658701026,
4.89206710306723));
#27255=CARTESIAN_POINT('Ctrl Pts',(-59.4904109039448,-4.24793472784974,
4.23556933641632));
#27256=CARTESIAN_POINT('Ctrl Pts',(-59.4439913559172,-4.81982763361711,
3.43270692109267));
#27257=CARTESIAN_POINT('Ctrl Pts',(-59.3975718078896,-5.39172053938448,
2.62984450576901));
#27258=CARTESIAN_POINT('Ctrl Pts',(-59.3511522598619,-5.75859821007974,
1.68061744177261));
#27259=CARTESIAN_POINT('Ctrl Pts',(-59.3047327118343,-5.87551327073906,
0.701680759602287));
#27260=CARTESIAN_POINT('Ctrl Pts',(-59.2936968719578,-5.90330879963607,
0.468947160661655));
#27261=CARTESIAN_POINT('Ctrl Pts',(-59.2826610320813,-5.9169762201901,0.234534347760465));
#27262=CARTESIAN_POINT('Ctrl Pts',(-59.2716251922048,-5.91673468093559,
9.87673099418387E-5));
#27263=CARTESIAN_POINT('Origin',(-29.75,0.,0.));
#27264=CARTESIAN_POINT('',(-57.2698748077951,-5.91669521102349,-0.000155415116674662));
#27265=CARTESIAN_POINT('',(-57.5216251922048,-5.91686007623345,-0.000149468482956774));
#27266=CARTESIAN_POINT('',(-29.75,-5.91675,-7.2459289488551E-16));
#27267=CARTESIAN_POINT('Ctrl Pts',(-57.2698748077951,-5.91669521102349,
-0.000155415116674662));
#27268=CARTESIAN_POINT('Ctrl Pts',(-57.3047703259064,-5.91594092446023,
0.741150481904227));
#27269=CARTESIAN_POINT('Ctrl Pts',(-57.3396658440178,-5.77622172722126,
1.48273266306714));
#27270=CARTESIAN_POINT('Ctrl Pts',(-57.3745613621291,-5.50418014344905,
2.17209688647092));
#27271=CARTESIAN_POINT('Ctrl Pts',(-57.4209809101567,-5.1422985022843,3.08911939849433));
#27272=CARTESIAN_POINT('Ctrl Pts',(-57.4674004581843,-4.5462659573424,3.91373969254815));
#27273=CARTESIAN_POINT('Ctrl Pts',(-57.5138200062119,-3.78904530466483,
4.54501260817227));
#27274=CARTESIAN_POINT('Ctrl Pts',(-57.5602395542395,-3.03182465198727,
5.17628552379639));
#27275=CARTESIAN_POINT('Ctrl Pts',(-57.6066591022671,-2.11341589157402,
5.61421106099084));
#27276=CARTESIAN_POINT('Ctrl Pts',(-57.6530786502948,-1.14624521793713,
5.80518094870228));
#27277=CARTESIAN_POINT('Ctrl Pts',(-57.6994981983224,-0.179074544300242,
5.99615083641373));
#27278=CARTESIAN_POINT('Ctrl Pts',(-57.74591774635,0.836858042560288,5.94016507464217));
#27279=CARTESIAN_POINT('Ctrl Pts',(-57.7923372943776,1.77718805466837,5.64407711940241));
#27280=CARTESIAN_POINT('Ctrl Pts',(-57.8387568424052,2.71751806677645,5.34798916416265));
#27281=CARTESIAN_POINT('Ctrl Pts',(-57.8851763904328,3.58224550413209,4.8117990154547));
#27282=CARTESIAN_POINT('Ctrl Pts',(-57.9315959384604,4.26551552444564,4.10114389853271));
#27283=CARTESIAN_POINT('Ctrl Pts',(-57.9780154864881,4.94878554475919,3.39048878161072));
#27284=CARTESIAN_POINT('Ctrl Pts',(-58.0244350345156,5.45059814803065,2.5053686964747));
#27285=CARTESIAN_POINT('Ctrl Pts',(-58.0708545825433,5.70952438737617,1.55413486686007));
#27286=CARTESIAN_POINT('Ctrl Pts',(-58.1172741305709,5.9684506267217,0.602901037245434));
#27287=CARTESIAN_POINT('Ctrl Pts',(-58.1636936785985,5.98449050214128,-0.414446536847809));
#27288=CARTESIAN_POINT('Ctrl Pts',(-58.2101132266261,5.75568050969606,-1.37337021725454));
#27289=CARTESIAN_POINT('Ctrl Pts',(-58.2565327746537,5.52687051725085,-2.33229389766127));
#27290=CARTESIAN_POINT('Ctrl Pts',(-58.3029523226813,5.05321065694084,-3.23279368438148));
#27291=CARTESIAN_POINT('Ctrl Pts',(-58.3493718707089,4.39268357467904,-3.96463556937447));
#27292=CARTESIAN_POINT('Ctrl Pts',(-58.3957914187365,3.73215649241724,-4.69647745436745));
#27293=CARTESIAN_POINT('Ctrl Pts',(-58.4422109667642,2.88476218820364,-5.2596614376332));
#27294=CARTESIAN_POINT('Ctrl Pts',(-58.4886305147918,1.95423369721252,-5.58524609364036));
#27295=CARTESIAN_POINT('Ctrl Pts',(-58.5350500628194,1.0237052062214,-5.91083074964752));
#27296=CARTESIAN_POINT('Ctrl Pts',(-58.581469610847,0.0100425284527469,
-5.99881607839609));
#27297=CARTESIAN_POINT('Ctrl Pts',(-58.6278891588746,-0.962667741224851,
-5.83843096005687));
#27298=CARTESIAN_POINT('Ctrl Pts',(-58.6743087069022,-1.93537801090245,
-5.67804584171765));
#27299=CARTESIAN_POINT('Ctrl Pts',(-58.7207282549299,-2.867135872489,-5.26929027629065));
#27300=CARTESIAN_POINT('Ctrl Pts',(-58.7671478029575,-3.64388096648873,
-4.66220263851837));
#27301=CARTESIAN_POINT('Ctrl Pts',(-58.8135673509851,-4.42062606048846,
-4.05511500074609));
#27302=CARTESIAN_POINT('Ctrl Pts',(-58.8599868990127,-5.04235838690136,
-3.24969529062854));
#27303=CARTESIAN_POINT('Ctrl Pts',(-58.9064064470403,-5.43296922428961,
-2.34453644495641));
#27304=CARTESIAN_POINT('Ctrl Pts',(-58.9442292339585,-5.75124010580946,
-1.60701030345509));
#27305=CARTESIAN_POINT('Ctrl Pts',(-58.9820520208768,-5.91606852332821,
-0.803266958259637));
#27306=CARTESIAN_POINT('Ctrl Pts',(-59.0198748077951,-5.9168929925076,0.000147316400840244));
#27307=CARTESIAN_POINT('Ctrl Pts',(-59.2716251922048,-5.91673468093559,
9.87673099418387E-5));
#27308=CARTESIAN_POINT('Ctrl Pts',(-59.2362414840537,-5.91596024468205,
-0.751561301314473));
#27309=CARTESIAN_POINT('Ctrl Pts',(-59.2008577759026,-5.77220078208614,
-1.50345542185119));
#27310=CARTESIAN_POINT('Ctrl Pts',(-59.1654740677515,-5.49267953958377,
-2.20098628354733));
#27311=CARTESIAN_POINT('Ctrl Pts',(-59.1190545197239,-5.12597829714577,
-3.1160703441824));
#27312=CARTESIAN_POINT('Ctrl Pts',(-59.0726349716963,-4.52562336164638,
-3.93759216510828));
#27313=CARTESIAN_POINT('Ctrl Pts',(-59.0262154236687,-3.76509506266973,
-4.56488611193625));
#27314=CARTESIAN_POINT('Ctrl Pts',(-58.979795875641,-3.00456676369308,-5.19218005876421));
#27315=CARTESIAN_POINT('Ctrl Pts',(-58.9333763276134,-2.08386510123916,
-5.62524613149425));
#27316=CARTESIAN_POINT('Ctrl Pts',(-58.8869567795858,-1.11570292286205,
-5.81112178033337));
#27317=CARTESIAN_POINT('Ctrl Pts',(-58.8405372315582,-0.147540744484937,
-5.99699742917248));
#27318=CARTESIAN_POINT('Ctrl Pts',(-58.7941176835306,0.868081949815372,
-5.93568265412068));
#27319=CARTESIAN_POINT('Ctrl Pts',(-58.747698135503,1.8068416706146,-5.63465720893411));
#27320=CARTESIAN_POINT('Ctrl Pts',(-58.7012785874754,2.74560139141385,-5.33363176374754));
#27321=CARTESIAN_POINT('Ctrl Pts',(-58.6548590394477,3.60749813871201,-4.79289564842621));
#27322=CARTESIAN_POINT('Ctrl Pts',(-58.6084394914201,4.28702201532277,-4.07865594235945));
#27323=CARTESIAN_POINT('Ctrl Pts',(-58.5620199433925,4.96654589193352,-3.36441623629269));
#27324=CARTESIAN_POINT('Ctrl Pts',(-58.5156003953649,5.46369689785686,-2.47667293948052));
#27325=CARTESIAN_POINT('Ctrl Pts',(-58.4691808473373,5.7176175382941,-1.52409151899249));
#27326=CARTESIAN_POINT('Ctrl Pts',(-58.4227612993097,5.97153817873133,-0.571510098504466));
#27327=CARTESIAN_POINT('Ctrl Pts',(-58.3763417512821,5.98222845368246,0.445909445659409));
#27328=CARTESIAN_POINT('Ctrl Pts',(-58.3299222032545,5.74837930985091,1.40361709377507));
#27329=CARTESIAN_POINT('Ctrl Pts',(-58.2835026552269,5.51453016601937,2.36132474189074));
#27330=CARTESIAN_POINT('Ctrl Pts',(-58.2370831071992,5.03614160340517,3.25932049395819));
#27331=CARTESIAN_POINT('Ctrl Pts',(-58.1906635591716,4.37177534567143,3.98767879377327));
#27332=CARTESIAN_POINT('Ctrl Pts',(-58.144244011144,3.70740908793767,4.71603709358836));
#27333=CARTESIAN_POINT('Ctrl Pts',(-58.0978244631164,2.85706513508438,5.27475794115106));
#27334=CARTESIAN_POINT('Ctrl Pts',(-58.0514049150888,1.92483748024982,5.59544509705575));
#27335=CARTESIAN_POINT('Ctrl Pts',(-58.0049853670612,0.992609825415271,
5.91613225296045));
#27336=CARTESIAN_POINT('Ctrl Pts',(-57.9585658190336,-0.0215015314005408,
5.99878571720714));
#27337=CARTESIAN_POINT('Ctrl Pts',(-57.912146271006,-0.993354991301984,
5.83328801179188));
#27338=CARTESIAN_POINT('Ctrl Pts',(-57.8657267229784,-1.96520845120343,
5.66779030637661));
#27339=CARTESIAN_POINT('Ctrl Pts',(-57.8193071749508,-2.89480401419051,
5.2541414312994));
#27340=CARTESIAN_POINT('Ctrl Pts',(-57.7728876269231,-3.66834609151454,
4.6429776048486));
#27341=CARTESIAN_POINT('Ctrl Pts',(-57.7264680788955,-4.44188816883857,
4.0318137783978));
#27342=CARTESIAN_POINT('Ctrl Pts',(-57.6800485308679,-5.05937676049954,
3.22313500057342));
#27343=CARTESIAN_POINT('Ctrl Pts',(-57.6336289828403,-5.44522253300335,
2.31593509171118));
#27344=CARTESIAN_POINT('Ctrl Pts',(-57.5962943859618,-5.75555292150966,
1.586286822292));
#27345=CARTESIAN_POINT('Ctrl Pts',(-57.5589597890833,-5.91603910242325,
0.79290758609723));
#27346=CARTESIAN_POINT('Ctrl Pts',(-57.5216251922048,-5.91686007623345,
-0.000149468482956774));
#27347=CARTESIAN_POINT('Origin',(-29.75,0.,0.));
#27348=CARTESIAN_POINT('',(-55.5198748077951,-5.91649353122104,0.000138118266801851));
#27349=CARTESIAN_POINT('',(-55.7716251922049,-5.91637209757686,0.000108738722670239));
#27350=CARTESIAN_POINT('',(-29.75,-5.91675,-7.2459289488551E-16));
#27351=CARTESIAN_POINT('Ctrl Pts',(-55.5198748077951,-5.91649353122104,
0.000138118266801851));
#27352=CARTESIAN_POINT('Ctrl Pts',(-55.5346495348808,-5.91676214941988,
0.314037003843105));
#27353=CARTESIAN_POINT('Ctrl Pts',(-55.5494242619665,-5.8922161605167,0.627894292230318));
#27354=CARTESIAN_POINT('Ctrl Pts',(-55.5641989890522,-5.84249117704565,
0.937710392677676));
#27355=CARTESIAN_POINT('Ctrl Pts',(-55.6106185370798,-5.68626417907686,
1.91109712740557));
#27356=CARTESIAN_POINT('Ctrl Pts',(-55.6570380851074,-5.28149433666472,
2.844593137236));
#27357=CARTESIAN_POINT('Ctrl Pts',(-55.703457633135,-4.67773119145832,3.62392533516499));
#27358=CARTESIAN_POINT('Ctrl Pts',(-55.7498771811627,-4.07396804625193,
4.40325753309398));
#27359=CARTESIAN_POINT('Ctrl Pts',(-55.7962967291902,-3.27121159825127,
5.02842591912155));
#27360=CARTESIAN_POINT('Ctrl Pts',(-55.8427162772178,-2.36773056682856,
5.42290105914683));
#27361=CARTESIAN_POINT('Ctrl Pts',(-55.8891358252455,-1.46424953540586,
5.81737619917211));
#27362=CARTESIAN_POINT('Ctrl Pts',(-55.9355553732731,-0.460043920561111,
5.98115809319512));
#27363=CARTESIAN_POINT('Ctrl Pts',(-55.9819749213007,0.521957337050214,
5.89419752576172));
#27364=CARTESIAN_POINT('Ctrl Pts',(-56.0283944693283,1.50395859466155,5.80723695832833));
#27365=CARTESIAN_POINT('Ctrl Pts',(-56.0748140173559,2.46375549503949,5.46953392943853));
#27366=CARTESIAN_POINT('Ctrl Pts',(-56.1212335653835,3.28385535096541,4.92242805618543));
#27367=CARTESIAN_POINT('Ctrl Pts',(-56.1676531134111,4.10395520689133,4.37532218293233));
#27368=CARTESIAN_POINT('Ctrl Pts',(-56.2140726614388,4.78435801836524,3.61881346531596));
#27369=CARTESIAN_POINT('Ctrl Pts',(-56.2604922094664,5.24177287803033,2.74550924776157));
#27370=CARTESIAN_POINT('Ctrl Pts',(-56.306911757494,5.69918773769542,1.87220503020718));
#27371=CARTESIAN_POINT('Ctrl Pts',(-56.3533313055216,5.93361464555165,0.882105312714779));
#27372=CARTESIAN_POINT('Ctrl Pts',(-56.3997508535492,5.91635643936607,-0.103587724976462));
#27373=CARTESIAN_POINT('Ctrl Pts',(-56.4461704015768,5.89909823318048,-1.08928076266769));
#27374=CARTESIAN_POINT('Ctrl Pts',(-56.4925899496044,5.63015491295308,-2.07056712055777));
#27375=CARTESIAN_POINT('Ctrl Pts',(-56.5390094976321,5.14244893695761,-2.92732349854667));
#27376=CARTESIAN_POINT('Ctrl Pts',(-56.5854290456597,4.65474296096214,-3.78407987653557));
#27377=CARTESIAN_POINT('Ctrl Pts',(-56.6318485936873,3.9482743291986,-4.5163062746233));
#27378=CARTESIAN_POINT('Ctrl Pts',(-56.6782681417149,3.10952477331956,-5.03436784697009));
#27379=CARTESIAN_POINT('Ctrl Pts',(-56.7246876897425,2.27077521744052,-5.55242941931689));
#27380=CARTESIAN_POINT('Ctrl Pts',(-56.7711072377701,1.29974473744598,-5.85632616592275));
#27381=CARTESIAN_POINT('Ctrl Pts',(-56.8175267857977,0.315301169254638,
-5.90885683587198));
#27382=CARTESIAN_POINT('Ctrl Pts',(-56.8639463338253,-0.669142398936689,
-5.96138750582122));
#27383=CARTESIAN_POINT('Ctrl Pts',(-56.910365881853,-1.66699905532482,-5.76255209911383));
#27384=CARTESIAN_POINT('Ctrl Pts',(-56.9567854298806,-2.55611706138655,
-5.33669087574605));
#27385=CARTESIAN_POINT('Ctrl Pts',(-57.0032049779082,-3.44523506744831,
-4.91082965237827));
#27386=CARTESIAN_POINT('Ctrl Pts',(-57.0496245259358,-4.22561442318367,
-4.25794261235009));
#27387=CARTESIAN_POINT('Ctrl Pts',(-57.0960440739634,-4.80172568112968,
-3.45795234453877));
#27388=CARTESIAN_POINT('Ctrl Pts',(-57.142463621991,-5.37783693907569,-2.65796207672745));
#27389=CARTESIAN_POINT('Ctrl Pts',(-57.1888831700186,-5.74968009923236,
-1.71086858113299));
#27390=CARTESIAN_POINT('Ctrl Pts',(-57.2353027180462,-5.87173631061688,
-0.732609468339251));
#27391=CARTESIAN_POINT('Ctrl Pts',(-57.2468267479625,-5.90203775669358,
-0.48974869608429));
#27392=CARTESIAN_POINT('Ctrl Pts',(-57.2583507778788,-5.91694430951495,
-0.244967121512084));
#27393=CARTESIAN_POINT('Ctrl Pts',(-57.2698748077951,-5.91669521102349,
-0.000155415116674662));
#27394=CARTESIAN_POINT('Ctrl Pts',(-57.5216251922048,-5.91686007623345,
-0.000149468482956774));
#27395=CARTESIAN_POINT('Ctrl Pts',(-57.5125402410557,-5.91705985090853,
-0.193130917372952));
#27396=CARTESIAN_POINT('Ctrl Pts',(-57.5034552899066,-5.90780525658231,
-0.3860932886948));
#27397=CARTESIAN_POINT('Ctrl Pts',(-57.4943703387574,-5.8889547826199,-0.578113641592445));
#27398=CARTESIAN_POINT('Ctrl Pts',(-57.4479507907298,-5.79263830638598,
-1.55924142613374));
#27399=CARTESIAN_POINT('Ctrl Pts',(-57.4015312427023,-5.4458024005715,-2.51577595531623));
#27400=CARTESIAN_POINT('Ctrl Pts',(-57.3551116946746,-4.89090467146282,
-3.33062386955801));
#27401=CARTESIAN_POINT('Ctrl Pts',(-57.308692146647,-4.33600694235414,-4.14547178379979));
#27402=CARTESIAN_POINT('Ctrl Pts',(-57.2622725986194,-3.57304738995126,
-4.81863308310086));
#27403=CARTESIAN_POINT('Ctrl Pts',(-57.2158530505918,-2.69542303387945,
-5.26770334013568));
#27404=CARTESIAN_POINT('Ctrl Pts',(-57.1694335025641,-1.81779867780764,
-5.71677359717049));
#27405=CARTESIAN_POINT('Ctrl Pts',(-57.1230139545365,-0.825509518066903,
-5.94175281193905));
#27406=CARTESIAN_POINT('Ctrl Pts',(-57.0765944065089,0.159974247990831,
-5.91510034460887));
#27407=CARTESIAN_POINT('Ctrl Pts',(-57.0301748584813,1.14545801404857,-5.88844787727869));
#27408=CARTESIAN_POINT('Ctrl Pts',(-56.9837553104537,2.12413638642329,-5.61016372784978));
#27409=CARTESIAN_POINT('Ctrl Pts',(-56.9373357624261,2.97620531871277,-5.11431380832405));
#27410=CARTESIAN_POINT('Ctrl Pts',(-56.8909162143985,3.82827425100224,-4.61846388879832));
#27411=CARTESIAN_POINT('Ctrl Pts',(-56.8444966663709,4.55373374320647,-3.90504819917577));
#27412=CARTESIAN_POINT('Ctrl Pts',(-56.7980771183432,5.06377731458045,-3.06139888678933));
#27413=CARTESIAN_POINT('Ctrl Pts',(-56.7516575703156,5.57382088595442,-2.21774957440287));
#27414=CARTESIAN_POINT('Ctrl Pts',(-56.7052380222881,5.86844853649814,-1.24386663925252));
#27415=CARTESIAN_POINT('Ctrl Pts',(-56.6588184742604,5.91159368326249,-0.25896709917957));
#27416=CARTESIAN_POINT('Ctrl Pts',(-56.6123989262328,5.95473883002684,0.725932440893382));
#27417=CARTESIAN_POINT('Ctrl Pts',(-56.5659793782052,5.74640147301182,1.72184858588893));
#27418=CARTESIAN_POINT('Ctrl Pts',(-56.5195598301776,5.31208504526766,2.60686714385153));
#27419=CARTESIAN_POINT('Ctrl Pts',(-56.47314028215,4.8777686175235,3.49188570181413));
#27420=CARTESIAN_POINT('Ctrl Pts',(-56.4267207341224,4.2174731190502,4.2660066727438));
#27421=CARTESIAN_POINT('Ctrl Pts',(-56.3803011860948,3.41202803826244,4.83446672352035));
#27422=CARTESIAN_POINT('Ctrl Pts',(-56.3338816380672,2.60658295747469,5.40292677429689));
#27423=CARTESIAN_POINT('Ctrl Pts',(-56.2874620900395,1.65598829437247,5.76572590492033));
#27424=CARTESIAN_POINT('Ctrl Pts',(-56.2410425420119,0.676610252469253,
5.8784523813965));
#27425=CARTESIAN_POINT('Ctrl Pts',(-56.1946229939843,-0.302767789433966,
5.99117885787268));
#27426=CARTESIAN_POINT('Ctrl Pts',(-56.1482034459567,-1.31092921013819,
5.85383268020161));
#27427=CARTESIAN_POINT('Ctrl Pts',(-56.1017838979291,-2.22446082252765,
5.48322695895988));
#27428=CARTESIAN_POINT('Ctrl Pts',(-56.0553643499015,-3.13799243491712,
5.11262123771814));
#27429=CARTESIAN_POINT('Ctrl Pts',(-56.0089448018738,-3.95689423899183,
4.50875597290575));
#27430=CARTESIAN_POINT('Ctrl Pts',(-55.9625252538462,-4.58092109591514,
3.74555279595537));
#27431=CARTESIAN_POINT('Ctrl Pts',(-55.9161057058186,-5.20494795283845,
2.98234961900499));
#27432=CARTESIAN_POINT('Ctrl Pts',(-55.8696861577911,-5.63409986261035,
2.05980852991662));
#27433=CARTESIAN_POINT('Ctrl Pts',(-55.8232666097634,-5.81584257440986,
1.09086157875583));
#27434=CARTESIAN_POINT('Ctrl Pts',(-55.8060528039106,-5.88323839985449,
0.73154604450996));
#27435=CARTESIAN_POINT('Ctrl Pts',(-55.7888389980577,-5.91661159960697,
0.365848980037442));
#27436=CARTESIAN_POINT('Ctrl Pts',(-55.7716251922049,-5.91637209757686,
0.000108738722670239));
#27437=CARTESIAN_POINT('Origin',(-29.75,0.,0.));
#27438=CARTESIAN_POINT('',(-53.7698748077951,-5.91709501868191,-0.000108451466299675));
#27439=CARTESIAN_POINT('',(-54.0216251922049,-5.91720758741406,-6.39274240385461E-5));
#27440=CARTESIAN_POINT('',(-29.75,-5.91675,-7.2459289488551E-16));
#27441=CARTESIAN_POINT('Ctrl Pts',(-53.7698748077951,-5.91709501868191,
-0.000108451466299675));
#27442=CARTESIAN_POINT('Ctrl Pts',(-53.8109482918828,-5.91635855568918,
0.872269577364956));
#27443=CARTESIAN_POINT('Ctrl Pts',(-53.8520217759704,-5.72101511215826,
1.74496643472829));
#27444=CARTESIAN_POINT('Ctrl Pts',(-53.8930952600581,-5.34756485588097,
2.53328917546711));
#27445=CARTESIAN_POINT('Ctrl Pts',(-53.9395148080857,-4.92550686659082,
3.42421883818736));
#27446=CARTESIAN_POINT('Ctrl Pts',(-53.9859343561134,-4.275960475547,4.20738096161857));
#27447=CARTESIAN_POINT('Ctrl Pts',(-54.032353904141,-3.47843932873723,4.78690544827096));
#27448=CARTESIAN_POINT('Ctrl Pts',(-54.0787734521686,-2.68091818192746,
5.36642993492334));
#27449=CARTESIAN_POINT('Ctrl Pts',(-54.1251930001962,-1.73542227935175,
5.74231678479689));
#27450=CARTESIAN_POINT('Ctrl Pts',(-54.1716125482238,-0.75769366425266,
5.86855214218494));
#27451=CARTESIAN_POINT('Ctrl Pts',(-54.2180320962514,0.220034950846445,
5.99478749957299));
#27452=CARTESIAN_POINT('Ctrl Pts',(-54.264451644279,1.22999627846893,5.87137136447552));
#27453=CARTESIAN_POINT('Ctrl Pts',(-54.3108711923066,2.14855679747888,5.51341161372878));
#27454=CARTESIAN_POINT('Ctrl Pts',(-54.3572907403343,3.06711731648883,5.15545186298203));
#27455=CARTESIAN_POINT('Ctrl Pts',(-54.4037102883619,3.89427702688625,4.56294849658601));
#27456=CARTESIAN_POINT('Ctrl Pts',(-54.4501298363895,4.52877990555298,3.808432289204));
#27457=CARTESIAN_POINT('Ctrl Pts',(-54.4965493844171,5.1632827842197,3.053916081822));
#27458=CARTESIAN_POINT('Ctrl Pts',(-54.5429689324447,5.60512883115574,2.13738703345401));
#27459=CARTESIAN_POINT('Ctrl Pts',(-54.5893884804723,5.80022985398318,1.17104123554823));
#27460=CARTESIAN_POINT('Ctrl Pts',(-54.6358080284999,5.99533087681063,0.20469543764244));
#27461=CARTESIAN_POINT('Ctrl Pts',(-54.6822275765276,5.94368687552949,-0.811467109801146));
#27462=CARTESIAN_POINT('Ctrl Pts',(-54.7286471245552,5.65161980480209,-1.75305376881625));
#27463=CARTESIAN_POINT('Ctrl Pts',(-54.7750666725828,5.35955273407469,-2.69464042783133));
#27464=CARTESIAN_POINT('Ctrl Pts',(-54.8214862206104,4.82706259390104,-3.56165119841793));
#27465=CARTESIAN_POINT('Ctrl Pts',(-54.867905768638,4.11933369302571,-4.24795172523127));
#27466=CARTESIAN_POINT('Ctrl Pts',(-54.9143253166656,3.41160479215037,-4.9342522520446));
#27467=CARTESIAN_POINT('Ctrl Pts',(-54.9607448646932,2.52863713057334,-5.43984253508467));
#27468=CARTESIAN_POINT('Ctrl Pts',(-55.0071644127209,1.57851841231285,-5.70283118778572));
#27469=CARTESIAN_POINT('Ctrl Pts',(-55.0535839607485,0.628399694052342,
-5.96581984048676));
#27470=CARTESIAN_POINT('Ctrl Pts',(-55.1000035087761,-0.388870080891639,
-5.98620686284878));
#27471=CARTESIAN_POINT('Ctrl Pts',(-55.1464230568037,-1.34876273427931,
-5.76149659559141));
#27472=CARTESIAN_POINT('Ctrl Pts',(-55.1928426048313,-2.30865538766697,
-5.53678632833405));
#27473=CARTESIAN_POINT('Ctrl Pts',(-55.2392621528589,-3.21117091949832,
-5.06697877145731));
#27474=CARTESIAN_POINT('Ctrl Pts',(-55.2856817008865,-3.9458286905366,-4.40958500080568));
#27475=CARTESIAN_POINT('Ctrl Pts',(-55.3321012489141,-4.68048646157487,
-3.75219123015404));
#27476=CARTESIAN_POINT('Ctrl Pts',(-55.3785207969418,-5.24728647182007,
-2.9072112457275));
#27477=CARTESIAN_POINT('Ctrl Pts',(-55.4249403449694,-5.57684440017996,
-1.97808252370154));
#27478=CARTESIAN_POINT('Ctrl Pts',(-55.4565851659113,-5.80150840653206,
-1.34468316309142));
#27479=CARTESIAN_POINT('Ctrl Pts',(-55.4882299868532,-5.91591819911813,
-0.672177110996802));
#27480=CARTESIAN_POINT('Ctrl Pts',(-55.5198748077951,-5.91649353122104,
0.000138118266801851));
#27481=CARTESIAN_POINT('Ctrl Pts',(-55.7716251922049,-5.91637209757686,
0.000108738722670239));
#27482=CARTESIAN_POINT('Ctrl Pts',(-55.7424194500301,-5.9159657473135,-0.620423134477549));
#27483=CARTESIAN_POINT('Ctrl Pts',(-55.7132137078553,-5.8188015680181,-1.24107929692855));
#27484=CARTESIAN_POINT('Ctrl Pts',(-55.6840079656806,-5.62688162061698,
-1.83090334586271));
#27485=CARTESIAN_POINT('Ctrl Pts',(-55.6375884176529,-5.32184444119746,
-2.76836850608727));
#27486=CARTESIAN_POINT('Ctrl Pts',(-55.5911688696254,-4.77743656853128,
-3.62794601330318));
#27487=CARTESIAN_POINT('Ctrl Pts',(-55.5447493215977,-4.0603012100281,-4.30441144852113));
#27488=CARTESIAN_POINT('Ctrl Pts',(-55.4983297735701,-3.34316585152493,
-4.98087688373906));
#27489=CARTESIAN_POINT('Ctrl Pts',(-55.4519102255425,-2.45330300718477,
-5.47423024695903));
#27490=CARTESIAN_POINT('Ctrl Pts',(-55.4054906775148,-1.4996444487146,-5.72407812331081));
#27491=CARTESIAN_POINT('Ctrl Pts',(-55.3590711294872,-0.545985890244415,
-5.97392599966261));
#27492=CARTESIAN_POINT('Ctrl Pts',(-55.3126515814597,0.471468382355783,
-5.98026838914621));
#27493=CARTESIAN_POINT('Ctrl Pts',(-55.2662320334321,1.42816760572891,-5.74232889377354));
#27494=CARTESIAN_POINT('Ctrl Pts',(-55.2198124854045,2.38486682910203,-5.50438939840087));
#27495=CARTESIAN_POINT('Ctrl Pts',(-55.1733929373768,3.28081100324809,-5.02216801817193));
#27496=CARTESIAN_POINT('Ctrl Pts',(-55.1269733893492,4.00632391585948,-4.35469545611802));
#27497=CARTESIAN_POINT('Ctrl Pts',(-55.0805538413215,4.73183682847088,-3.6872228940641));
#27498=CARTESIAN_POINT('Ctrl Pts',(-55.034134293294,5.28691847954762,-2.83449915018519));
#27499=CARTESIAN_POINT('Ctrl Pts',(-54.9877147452664,5.60361904055304,-1.90090964610978));
#27500=CARTESIAN_POINT('Ctrl Pts',(-54.9412951972388,5.92031960155846,-0.96732014203436));
#27501=CARTESIAN_POINT('Ctrl Pts',(-54.8948756492112,5.99863907249256,0.047135122237555));
#27502=CARTESIAN_POINT('Ctrl Pts',(-54.8484561011835,5.82899004470886,1.01827250429678));
#27503=CARTESIAN_POINT('Ctrl Pts',(-54.8020365531559,5.65934101692516,1.98940988635599));
#27504=CARTESIAN_POINT('Ctrl Pts',(-54.7556170051283,5.24172349042367,2.9172293862025));
#27505=CARTESIAN_POINT('Ctrl Pts',(-54.7091974571007,4.62725974471876,3.68815280177316));
#27506=CARTESIAN_POINT('Ctrl Pts',(-54.6627779090731,4.01279599901386,4.45907621734382));
#27507=CARTESIAN_POINT('Ctrl Pts',(-54.6163583610455,3.20148603410555,5.07310354863862));
#27508=CARTESIAN_POINT('Ctrl Pts',(-54.5699388130179,2.29264564056018,5.45506918390062));
#27509=CARTESIAN_POINT('Ctrl Pts',(-54.5235192649903,1.3838052470148,5.83703481916262));
#27510=CARTESIAN_POINT('Ctrl Pts',(-54.4770997169626,0.377434424832348,
5.98693875839182));
#27511=CARTESIAN_POINT('Ctrl Pts',(-54.430680168935,-0.603272833393652,
5.88643064367627));
#27512=CARTESIAN_POINT('Ctrl Pts',(-54.3842606209074,-1.58398009161965,
5.78592252896073));
#27513=CARTESIAN_POINT('Ctrl Pts',(-54.3378410728798,-2.53902378588921,
5.43500236030046));
#27514=CARTESIAN_POINT('Ctrl Pts',(-54.2914215248522,-3.3514930884985,4.87662771924089));
#27515=CARTESIAN_POINT('Ctrl Pts',(-54.2450019768246,-4.16396239110779,
4.31825307818133));
#27516=CARTESIAN_POINT('Ctrl Pts',(-54.198582428797,-4.83385730205682,3.55242396472248));
#27517=CARTESIAN_POINT('Ctrl Pts',(-54.1521628807693,-5.27917322932164,
2.6728886712947));
#27518=CARTESIAN_POINT('Ctrl Pts',(-54.1086503179145,-5.69660162099499,
1.84843353623915));
#27519=CARTESIAN_POINT('Ctrl Pts',(-54.0651377550597,-5.9166984185426,0.924067797853219));
#27520=CARTESIAN_POINT('Ctrl Pts',(-54.0216251922049,-5.91720758741406,
-6.39274240385461E-5));
#27521=CARTESIAN_POINT('Origin',(-29.75,0.,0.));
#27522=CARTESIAN_POINT('',(-52.0198748077951,-5.91625820056289,4.45556367170696E-5));
#27523=CARTESIAN_POINT('',(-52.2716251922048,-5.91623884227222,-3.64161732908164E-6));
#27524=CARTESIAN_POINT('',(-29.75,-5.91675,-7.2459289488551E-16));
#27525=CARTESIAN_POINT('Ctrl Pts',(-52.0198748077951,-5.91625820056289,
4.45556367170696E-5));
#27526=CARTESIAN_POINT('Ctrl Pts',(-52.0408275008571,-5.91637479742008,
0.445249139576727));
#27527=CARTESIAN_POINT('Ctrl Pts',(-52.0617801939192,-5.86678403741804,
0.890428155919709));
#27528=CARTESIAN_POINT('Ctrl Pts',(-52.0827328869812,-5.7672074757706,1.32413060753377));
#27529=CARTESIAN_POINT('Ctrl Pts',(-52.1291524350089,-5.54660103763264,
2.28497472063982));
#27530=CARTESIAN_POINT('Ctrl Pts',(-52.1755719830365,-5.08065436583636,
3.18948957664679));
#27531=CARTESIAN_POINT('Ctrl Pts',(-52.2219915310641,-4.42640590939973,
3.92694979082025));
#27532=CARTESIAN_POINT('Ctrl Pts',(-52.2684110790917,-3.7721574529631,4.66441000499372));
#27533=CARTESIAN_POINT('Ctrl Pts',(-52.3148306271193,-2.92960721188612,
5.23481557733369));
#27534=CARTESIAN_POINT('Ctrl Pts',(-52.3612501751469,-2.0018952274647,5.56834081505848));
#27535=CARTESIAN_POINT('Ctrl Pts',(-52.4076697231746,-1.07418324304329,
5.90186605278327));
#27536=CARTESIAN_POINT('Ctrl Pts',(-52.4540892712022,-0.0613095152774347,
5.99851095589289));
#27537=CARTESIAN_POINT('Ctrl Pts',(-52.5005088192298,0.912735915813663,
5.84644482419666));
#27538=CARTESIAN_POINT('Ctrl Pts',(-52.5469283672574,1.88678134690476,5.69437869250042));
#27539=CARTESIAN_POINT('Ctrl Pts',(-52.593347915285,2.82199848132111,5.29360152599834));
#27540=CARTESIAN_POINT('Ctrl Pts',(-52.6397674633126,3.60390354211778,4.69317410645535));
#27541=CARTESIAN_POINT('Ctrl Pts',(-52.6861870113402,4.38580860291444,4.09274668691237));
#27542=CARTESIAN_POINT('Ctrl Pts',(-52.7326065593678,5.01440159009144,3.29266901432849));
#27543=CARTESIAN_POINT('Ctrl Pts',(-52.7790261073954,5.41273385003153,2.39088188815653));
#27544=CARTESIAN_POINT('Ctrl Pts',(-52.825445655423,5.81106610997162,1.48909476198456));
#27545=CARTESIAN_POINT('Ctrl Pts',(-52.8718652034507,5.9791376426748,0.485598182224505));
#27546=CARTESIAN_POINT('Ctrl Pts',(-52.9182847514783,5.89637412036982,-0.496765706369812));
#27547=CARTESIAN_POINT('Ctrl Pts',(-52.9647042995059,5.81361059806484,-1.47912959496415));
#27548=CARTESIAN_POINT('Ctrl Pts',(-53.0111238475335,5.48001202075168,-2.44036079239273));
#27549=CARTESIAN_POINT('Ctrl Pts',(-53.0575433955611,4.93641556271725,-3.26279103323443));
#27550=CARTESIAN_POINT('Ctrl Pts',(-53.1039629435887,4.39281910468283,-4.08522127407612));
#27551=CARTESIAN_POINT('Ctrl Pts',(-53.1503824916163,3.63922476592713,-4.76885055833092));
#27552=CARTESIAN_POINT('Ctrl Pts',(-53.196802039644,2.76788312977477,-5.22999301283475));
#27553=CARTESIAN_POINT('Ctrl Pts',(-53.2432215876716,1.89654149362241,-5.69113546733857));
#27554=CARTESIAN_POINT('Ctrl Pts',(-53.2896411356992,0.90745256007338,-5.92979109209143));
#27555=CARTESIAN_POINT('Ctrl Pts',(-53.3360606837268,-0.0783052253648198,
-5.91674507022845));
#27556=CARTESIAN_POINT('Ctrl Pts',(-53.3824802317544,-1.06406301080302,
-5.90369904836547));
#27557=CARTESIAN_POINT('Ctrl Pts',(-53.428899779782,-2.04648964813039,-5.63895137988666));
#27558=CARTESIAN_POINT('Ctrl Pts',(-53.4753193278097,-2.90532225092888,
-5.1549109160731));
#27559=CARTESIAN_POINT('Ctrl Pts',(-53.5217388758373,-3.76415485372738,
-4.67087045225953));
#27560=CARTESIAN_POINT('Ctrl Pts',(-53.5681584238649,-4.49939342199699,
-3.96753719311121));
#27561=CARTESIAN_POINT('Ctrl Pts',(-53.6145779718925,-5.02103437779471,
-3.13100905642186));
#27562=CARTESIAN_POINT('Ctrl Pts',(-53.6609975199201,-5.54267533359243,
-2.29448091973252));
#27563=CARTESIAN_POINT('Ctrl Pts',(-53.7074170679477,-5.85071867691826,
-1.32475790550216));
#27564=CARTESIAN_POINT('Ctrl Pts',(-53.7538366159753,-5.90745555481293,
-0.340547797382322));
#27565=CARTESIAN_POINT('Ctrl Pts',(-53.7591826799153,-5.91398984887363,
-0.227197918033964));
#27566=CARTESIAN_POINT('Ctrl Pts',(-53.7645287438552,-5.91719087561579,
-0.113655885425565));
#27567=CARTESIAN_POINT('Ctrl Pts',(-53.7698748077951,-5.91709501868191,
-0.000108451466299675));
#27568=CARTESIAN_POINT('Ctrl Pts',(-54.0216251922049,-5.91720758741406,
-6.39274240385461E-5));
#27569=CARTESIAN_POINT('Ctrl Pts',(-54.0187182070321,-5.91724160394314,
-0.061803274564678));
#27570=CARTESIAN_POINT('Ctrl Pts',(-54.0158112218593,-5.91629553449657,
-0.123541577234064));
#27571=CARTESIAN_POINT('Ctrl Pts',(-54.0129042366865,-5.91436274267908,
-0.185248973901452));
#27572=CARTESIAN_POINT('Ctrl Pts',(-53.9664846886589,-5.88349938519108,
-1.17060985227313));
#27573=CARTESIAN_POINT('Ctrl Pts',(-53.9200651406313,-5.60103572663448,
-2.14809013561975));
#27574=CARTESIAN_POINT('Ctrl Pts',(-53.8736455926037,-5.10154930552007,
-2.99803244106357));
#27575=CARTESIAN_POINT('Ctrl Pts',(-53.8272260445761,-4.60206288440565,
-3.84797474650739));
#27576=CARTESIAN_POINT('Ctrl Pts',(-53.7808064965484,-3.88555370073343,
-4.5703790740484));
#27577=CARTESIAN_POINT('Ctrl Pts',(-53.7343869485208,-3.03973259142438,
-5.07681293795175));
#27578=CARTESIAN_POINT('Ctrl Pts',(-53.6879674004932,-2.19391148211535,
-5.58324680185509));
#27579=CARTESIAN_POINT('Ctrl Pts',(-53.6415478524656,-1.2187784471695,-5.87371020212078));
#27580=CARTESIAN_POINT('Ctrl Pts',(-53.595128304438,-0.233703533131209,
-5.91264631894415));
#27581=CARTESIAN_POINT('Ctrl Pts',(-53.5487087564104,0.751371380907081,
-5.95158243576752));
#27582=CARTESIAN_POINT('Ctrl Pts',(-53.5022892083828,1.74638817403782,-5.73899126914857));
#27583=CARTESIAN_POINT('Ctrl Pts',(-53.4558696603552,2.62954274707465,-5.30089697840176));
#27584=CARTESIAN_POINT('Ctrl Pts',(-53.4094501123276,3.51269732011148,-4.86280268765496));
#27585=CARTESIAN_POINT('Ctrl Pts',(-53.3630305642999,4.2839896730544,-4.19920527278031));
#27586=CARTESIAN_POINT('Ctrl Pts',(-53.3166110162723,4.84900273585183,-3.39133842339913));
#27587=CARTESIAN_POINT('Ctrl Pts',(-53.2701914682447,5.41401579864927,-2.58347157401794));
#27588=CARTESIAN_POINT('Ctrl Pts',(-53.2237719202171,5.77274957130122,-1.63133529013022));
#27589=CARTESIAN_POINT('Ctrl Pts',(-53.1773523721895,5.88128997685213,-0.651484491373765));
#27590=CARTESIAN_POINT('Ctrl Pts',(-53.1309328241619,5.98983038240304,0.328366307382695));
#27591=CARTESIAN_POINT('Ctrl Pts',(-53.0845132761342,5.84817742085291,1.33593162100792));
#27592=CARTESIAN_POINT('Ctrl Pts',(-53.0380937281066,5.4736714139911,2.24787123429668));
#27593=CARTESIAN_POINT('Ctrl Pts',(-52.991674180079,5.09916540712929,3.15981084758544));
#27594=CARTESIAN_POINT('Ctrl Pts',(-52.9452546320514,4.49180635495582,3.97612476053773));
#27595=CARTESIAN_POINT('Ctrl Pts',(-52.8988350840238,3.72594357774684,4.59688462872073));
#27596=CARTESIAN_POINT('Ctrl Pts',(-52.8524155359962,2.96008080053786,5.21764449690374));
#27597=CARTESIAN_POINT('Ctrl Pts',(-52.8059959879686,2.03571429829339,5.64285032031743));
#27598=CARTESIAN_POINT('Ctrl Pts',(-52.759576439941,1.06599957743425,5.82045090480384));
#27599=CARTESIAN_POINT('Ctrl Pts',(-52.7131568919134,0.0962848565751215,
5.99805148929024));
#27600=CARTESIAN_POINT('Ctrl Pts',(-52.6667373438857,-0.918778082898684,
5.92804683484937));
#27601=CARTESIAN_POINT('Ctrl Pts',(-52.6203177958581,-1.85493121055628,
5.6190064992333));
#27602=CARTESIAN_POINT('Ctrl Pts',(-52.5738982478305,-2.79108433821389,
5.30996616361722));
#27603=CARTESIAN_POINT('Ctrl Pts',(-52.5274786998029,-3.6483276540553,4.76189014682594));
#27604=CARTESIAN_POINT('Ctrl Pts',(-52.4810591517753,-4.3217224770548,4.04187068888172));
#27605=CARTESIAN_POINT('Ctrl Pts',(-52.4346396037477,-4.9951173000543,3.32185123093749));
#27606=CARTESIAN_POINT('Ctrl Pts',(-52.38822005572,-5.48466363021188,2.42988833184032));
#27607=CARTESIAN_POINT('Ctrl Pts',(-52.3418005076924,-5.7304340872396,1.47517083964002));
#27608=CARTESIAN_POINT('Ctrl Pts',(-52.3184087358632,-5.85428291165581,
0.994068918406044));
#27609=CARTESIAN_POINT('Ctrl Pts',(-52.295016964034,-5.91622824475799,0.497031341361674));
#27610=CARTESIAN_POINT('Ctrl Pts',(-52.2716251922048,-5.91623884227222,
-3.64161732908164E-6));
#27611=CARTESIAN_POINT('Origin',(-29.75,0.,0.));
#27612=CARTESIAN_POINT('',(-50.2698748077951,-5.91725823033598,1.89064590639526E-5));
#27613=CARTESIAN_POINT('',(-50.5216251922048,-5.91719392214832,7.12702798121252E-5));
#27614=CARTESIAN_POINT('',(-29.75,-5.91675,-7.2459289488551E-16));
#27615=CARTESIAN_POINT('Ctrl Pts',(-50.2698748077951,-5.91725823033598,
1.89064590639526E-5));
#27616=CARTESIAN_POINT('Ctrl Pts',(-50.2707067098315,-5.91726143750099,
0.0176866299085558));
#27617=CARTESIAN_POINT('Ctrl Pts',(-50.271538611868,-5.9171839715363,0.0353543251200561));
#27618=CARTESIAN_POINT('Ctrl Pts',(-50.2723705139044,-5.91702566130763,
0.0530212959021068));
#27619=CARTESIAN_POINT('Ctrl Pts',(-50.318790061932,-5.90819206198753,1.03882582914462));
#27620=CARTESIAN_POINT('Ctrl Pts',(-50.3652096099596,-5.64764487955008,
2.0223748067859));
#27621=CARTESIAN_POINT('Ctrl Pts',(-50.4116291579872,-5.16727876649904,
2.88326795211271));
#27622=CARTESIAN_POINT('Ctrl Pts',(-50.4580487060148,-4.68691265344798,
3.74416109743955));
#27623=CARTESIAN_POINT('Ctrl Pts',(-50.5044682540424,-3.98672760978333,
4.48239841045192));
#27624=CARTESIAN_POINT('Ctrl Pts',(-50.55088780207,-3.15243616728958,5.00760922452588));
#27625=CARTESIAN_POINT('Ctrl Pts',(-50.5973073500976,-2.31814472479584,
5.53282003859983));
#27626=CARTESIAN_POINT('Ctrl Pts',(-50.6437268981253,-1.34974688347302,
5.84500435373537));
#27627=CARTESIAN_POINT('Ctrl Pts',(-50.6901464461529,-0.365788207105206,
5.90594640357791));
#27628=CARTESIAN_POINT('Ctrl Pts',(-50.7365659941805,0.618170469262604,
5.96688845342044));
#27629=CARTESIAN_POINT('Ctrl Pts',(-50.7829855422081,1.6176899806754,5.77658823796997));
#27630=CARTESIAN_POINT('Ctrl Pts',(-50.8294050902357,2.51041503167754,5.35834118950254));
#27631=CARTESIAN_POINT('Ctrl Pts',(-50.8758246382633,3.40314008267966,4.94009414103513));
#27632=CARTESIAN_POINT('Ctrl Pts',(-50.9222441862909,4.18907067327115,4.29390025955077));
#27633=CARTESIAN_POINT('Ctrl Pts',(-50.9686637343185,4.77199780650754,3.49886279654966));
#27634=CARTESIAN_POINT('Ctrl Pts',(-51.0150832823462,5.35492493974395,2.70382533354852));
#27635=CARTESIAN_POINT('Ctrl Pts',(-51.0615028303738,5.73484861562527,1.75994428903063));
#27636=CARTESIAN_POINT('Ctrl Pts',(-51.1079223784014,5.86526081396552,0.782764024820095));
#27637=CARTESIAN_POINT('Ctrl Pts',(-51.154341926429,5.99567301230578,-0.194416239390436));
#27638=CARTESIAN_POINT('Ctrl Pts',(-51.2007614744566,5.87657373310498,-1.2048957232936));
#27639=CARTESIAN_POINT('Ctrl Pts',(-51.2471810224842,5.52254240910932,-2.12497747611146));
#27640=CARTESIAN_POINT('Ctrl Pts',(-51.2936005705118,5.16851108511367,-3.04505922892933));
#27641=CARTESIAN_POINT('Ctrl Pts',(-51.3400201185395,4.57954771632317,-3.87474325066188));
#27642=CARTESIAN_POINT('Ctrl Pts',(-51.3864396665671,3.82774973173052,-4.51246450685531));
#27643=CARTESIAN_POINT('Ctrl Pts',(-51.4328592145947,3.07595174713789,-5.15018576304874));
#27644=CARTESIAN_POINT('Ctrl Pts',(-51.4792787626223,2.1613191467431,-5.59594425370305));
#27645=CARTESIAN_POINT('Ctrl Pts',(-51.5256983106499,1.19581586999591,-5.79517284810884));
#27646=CARTESIAN_POINT('Ctrl Pts',(-51.5721178586775,0.230312593248732,
-5.99440144251464));
#27647=CARTESIAN_POINT('Ctrl Pts',(-51.6185374067051,-0.786061359850855,
-5.94710014067192));
#27648=CARTESIAN_POINT('Ctrl Pts',(-51.6649569547327,-1.7288874723005,-5.65905928953872));
#27649=CARTESIAN_POINT('Ctrl Pts',(-51.7113765027604,-2.67171358475018,
-5.37101843840551));
#27650=CARTESIAN_POINT('Ctrl Pts',(-51.757796050788,-3.54099185654992,-4.84223803798179));
#27651=CARTESIAN_POINT('Ctrl Pts',(-51.8042155988156,-4.23031035820282,
-4.13744827250734));
#27652=CARTESIAN_POINT('Ctrl Pts',(-51.8506351468432,-4.91962885985571,
-3.4326585070329));
#27653=CARTESIAN_POINT('Ctrl Pts',(-51.8970546948708,-5.42898759136177,
-2.55185937650774));
#27654=CARTESIAN_POINT('Ctrl Pts',(-51.9434742428984,-5.69603385487499,
-1.60287312614258));
#27655=CARTESIAN_POINT('Ctrl Pts',(-51.968941097864,-5.84254171096053,-1.08223696682489));
#27656=CARTESIAN_POINT('Ctrl Pts',(-51.9944079528295,-5.91611648344602,
-0.541077319991566));
#27657=CARTESIAN_POINT('Ctrl Pts',(-52.0198748077951,-5.91625820056289,
4.45556367170696E-5));
#27658=CARTESIAN_POINT('Ctrl Pts',(-52.2716251922048,-5.91623884227222,
-3.64161732908164E-6));
#27659=CARTESIAN_POINT('Ctrl Pts',(-52.2485974160064,-5.91624927488023,
-0.489304342495949));
#27660=CARTESIAN_POINT('Ctrl Pts',(-52.225569639808,-5.85623748812403,-0.97860252941275));
#27661=CARTESIAN_POINT('Ctrl Pts',(-52.2025418636096,-5.73617367371246,
-1.45269247238703));
#27662=CARTESIAN_POINT('Ctrl Pts',(-52.156122315582,-5.49414821925973,-2.40836620691037));
#27663=CARTESIAN_POINT('Ctrl Pts',(-52.1097027675544,-5.0081027264564,-3.30224159065363));
#27664=CARTESIAN_POINT('Ctrl Pts',(-52.0632832195268,-4.33753602368729,
-4.02489566045343));
#27665=CARTESIAN_POINT('Ctrl Pts',(-52.0168636714992,-3.6669693209182,-4.74754973025321));
#27666=CARTESIAN_POINT('Ctrl Pts',(-51.9704441234715,-2.81188140818333,
-5.29898248610953));
#27667=CARTESIAN_POINT('Ctrl Pts',(-51.9240245754439,-1.87694711474672,
-5.61169077576142));
#27668=CARTESIAN_POINT('Ctrl Pts',(-51.8776050274163,-0.94201282131012,
-5.9243990654133));
#27669=CARTESIAN_POINT('Ctrl Pts',(-51.8311854793887,0.0727678528282248,
-5.99838288886075));
#27670=CARTESIAN_POINT('Ctrl Pts',(-51.7847659313611,1.0431714304984,-5.82458558190312));
#27671=CARTESIAN_POINT('Ctrl Pts',(-51.7383463833335,2.0135750081686,-5.6507882749455));
#27672=CARTESIAN_POINT('Ctrl Pts',(-51.6919268353059,2.93960148937063,-5.22920983758279));
#27673=CARTESIAN_POINT('Ctrl Pts',(-51.6455072872783,3.70789216283027,-4.61145742072327));
#27674=CARTESIAN_POINT('Ctrl Pts',(-51.5990877392506,4.47618283628991,-3.99370500386375));
#27675=CARTESIAN_POINT('Ctrl Pts',(-51.552668191223,5.08673770200714,-3.17977860750742));
#27676=CARTESIAN_POINT('Ctrl Pts',(-51.5062486431954,5.46481622702219,-2.26931431035827));
#27677=CARTESIAN_POINT('Ctrl Pts',(-51.4598290951678,5.84289475203723,-1.35885001320913));
#27678=CARTESIAN_POINT('Ctrl Pts',(-51.4134095471402,5.98849693635009,-0.351847815267173));
#27679=CARTESIAN_POINT('Ctrl Pts',(-51.3669899991126,5.88379901756576,0.628421001569855));
#27680=CARTESIAN_POINT('Ctrl Pts',(-51.320570451085,5.77910109878143,1.60868981840687));
#27681=CARTESIAN_POINT('Ctrl Pts',(-51.2741509030574,5.42410307689992,2.56222525413896));
#27682=CARTESIAN_POINT('Ctrl Pts',(-51.2277313550298,4.86226172025593,3.37230111319492));
#27683=CARTESIAN_POINT('Ctrl Pts',(-51.1813118070021,4.30042036361194,4.18237697225088));
#27684=CARTESIAN_POINT('Ctrl Pts',(-51.1348922589745,3.53173567220546,4.8489932546307));
#27685=CARTESIAN_POINT('Ctrl Pts',(-51.0884727109469,2.65030550151139,5.29054671872201));
#27686=CARTESIAN_POINT('Ctrl Pts',(-51.0420531629193,1.76887533081731,5.73210018281333));
#27687=CARTESIAN_POINT('Ctrl Pts',(-50.9956336148917,0.774699680835636,
5.94859082861613));
#27688=CARTESIAN_POINT('Ctrl Pts',(-50.9492140668641,-0.210520317040655,
5.91351714552642));
#27689=CARTESIAN_POINT('Ctrl Pts',(-50.9027945188365,-1.19574031491695,
5.87844346243672));
#27690=CARTESIAN_POINT('Ctrl Pts',(-50.8563749708089,-2.17200466068785,
5.59180545045453));
#27691=CARTESIAN_POINT('Ctrl Pts',(-50.8099554227812,-3.01980481939666,
5.08869164786692));
#27692=CARTESIAN_POINT('Ctrl Pts',(-50.7635358747536,-3.86760497810546,
4.58557784527932));
#27693=CARTESIAN_POINT('Ctrl Pts',(-50.717116326726,-4.58694094975216,3.86598825208632));
#27694=CARTESIAN_POINT('Ctrl Pts',(-50.6706967786984,-5.08975585867029,
3.01801079081128));
#27695=CARTESIAN_POINT('Ctrl Pts',(-50.6242772306708,-5.59257076758842,
2.17003332953624));
#27696=CARTESIAN_POINT('Ctrl Pts',(-50.5778576826432,-5.87886461377798,
1.19366800017916));
#27697=CARTESIAN_POINT('Ctrl Pts',(-50.5314381346156,-5.91359098970248,
0.208435699512988));
#27698=CARTESIAN_POINT('Ctrl Pts',(-50.528167153812,-5.91603800424384,0.139010724917649));
#27699=CARTESIAN_POINT('Ctrl Pts',(-50.5248961730084,-5.9172358858531,0.0695417222694849));
#27700=CARTESIAN_POINT('Ctrl Pts',(-50.5216251922048,-5.91719392214832,
7.12702798121252E-5));
#27701=CARTESIAN_POINT('Origin',(-29.75,0.,0.));
#27702=CARTESIAN_POINT('',(-48.5198748077951,-5.91629691922315,-7.52784257820883E-5));
#27703=CARTESIAN_POINT('',(-48.7716251922048,-5.91638811723421,-0.000113882446527966));
#27704=CARTESIAN_POINT('',(-29.75,-5.91675,-7.2459289488551E-16));
#27705=CARTESIAN_POINT('Ctrl Pts',(-48.5198748077951,-5.91629691922315,
-7.52784257820882E-5));
#27706=CARTESIAN_POINT('Ctrl Pts',(-48.5470054668335,-5.91603979408007,
0.576388453514846));
#27707=CARTESIAN_POINT('Ctrl Pts',(-48.5741361258719,-5.8323893316429,1.15292520994488));
#27708=CARTESIAN_POINT('Ctrl Pts',(-48.6012667849103,-5.66639543983512,
1.70468960629431));
#27709=CARTESIAN_POINT('Ctrl Pts',(-48.6476863329379,-5.38238606792292,
2.64873795617079));
#27710=CARTESIAN_POINT('Ctrl Pts',(-48.6941058809656,-4.85732506278092,
3.52026785615966));
#27711=CARTESIAN_POINT('Ctrl Pts',(-48.7405254289932,-4.1554873021707,4.21259174569411));
#27712=CARTESIAN_POINT('Ctrl Pts',(-48.7869449770208,-3.45364954156048,
4.90491563522857));
#27713=CARTESIAN_POINT('Ctrl Pts',(-48.8333645250484,-2.57503502548203,
5.41803351430862));
#27714=CARTESIAN_POINT('Ctrl Pts',(-48.879784073076,-1.62719857150409,5.6891325123684));
#27715=CARTESIAN_POINT('Ctrl Pts',(-48.9262036211036,-0.679362117526128,
5.96023151042818));
#27716=CARTESIAN_POINT('Ctrl Pts',(-48.9726231691312,0.337696274351328,
5.9893116274677));
#27717=CARTESIAN_POINT('Ctrl Pts',(-49.0190427171588,1.29947430215932,5.77281304672337));
#27718=CARTESIAN_POINT('Ctrl Pts',(-49.0654622651865,2.26125232996726,5.55631446597905));
#27719=CARTESIAN_POINT('Ctrl Pts',(-49.1118818132141,3.1677499937057,5.09423718745094));
#27720=CARTESIAN_POINT('Ctrl Pts',(-49.1583013612417,3.90799918498855,4.44314599180816));
#27721=CARTESIAN_POINT('Ctrl Pts',(-49.2047209092693,4.64824837627141,3.79205479616537));
#27722=CARTESIAN_POINT('Ctrl Pts',(-49.2511404572969,5.22224909509864,2.95194968340791));
#27723=CARTESIAN_POINT('Ctrl Pts',(-49.2975600053245,5.55973555201645,2.02567137661478));
#27724=CARTESIAN_POINT('Ctrl Pts',(-49.3439795533521,5.89722200893427,1.09939306982164));
#27725=CARTESIAN_POINT('Ctrl Pts',(-49.3903991013797,5.99819420394269,0.0869415689928164));
#27726=CARTESIAN_POINT('Ctrl Pts',(-49.4368186494074,5.85029171524704,-0.887744772388931));
#27727=CARTESIAN_POINT('Ctrl Pts',(-49.483238197435,5.7023892265514,-1.86243111377068));
#27728=CARTESIAN_POINT('Ctrl Pts',(-49.5296577454626,5.3056120541517,-2.79935229570535));
#27729=CARTESIAN_POINT('Ctrl Pts',(-49.5760772934902,4.70853132407867,-3.58381594178078));
#27730=CARTESIAN_POINT('Ctrl Pts',(-49.6224968415178,4.11145059400564,-4.36827958785621));
#27731=CARTESIAN_POINT('Ctrl Pts',(-49.6689163895454,3.31406630625929,-5.00028569807241));
#27732=CARTESIAN_POINT('Ctrl Pts',(-49.715335937573,2.41398955197377,-5.40246780437918));
#27733=CARTESIAN_POINT('Ctrl Pts',(-49.7617554856006,1.51391279768828,-5.80464991068593));
#27734=CARTESIAN_POINT('Ctrl Pts',(-49.8081750336282,0.511143576863623,
-5.97700801308327));
#27735=CARTESIAN_POINT('Ctrl Pts',(-49.8545945816558,-0.471565004746035,
-5.89844304716854));
#27736=CARTESIAN_POINT('Ctrl Pts',(-49.9010141296834,-1.45427358635572,
-5.81987808125382));
#27737=CARTESIAN_POINT('Ctrl Pts',(-49.9474336777111,-2.41692152875041,
-5.49039004702702));
#27738=CARTESIAN_POINT('Ctrl Pts',(-49.9938532257387,-3.24166713692909,
-4.95031293028491));
#27739=CARTESIAN_POINT('Ctrl Pts',(-50.0402727737663,-4.06641274510778,
-4.41023581354281));
#27740=CARTESIAN_POINT('Ctrl Pts',(-50.0866923217939,-4.75325601907047,
-3.65956961428539));
#27741=CARTESIAN_POINT('Ctrl Pts',(-50.1331118698215,-5.21811764795045,
-2.79020647023479));
#27742=CARTESIAN_POINT('Ctrl Pts',(-50.1786995158127,-5.67464831816857,
-1.93642350739356));
#27743=CARTESIAN_POINT('Ctrl Pts',(-50.2242871618039,-5.91708247995128,
-0.968159901647365));
#27744=CARTESIAN_POINT('Ctrl Pts',(-50.2698748077951,-5.91725823033598,
1.89064590639526E-5));
#27745=CARTESIAN_POINT('Ctrl Pts',(-50.5216251922048,-5.91719392214832,
7.12702798121252E-5));
#27746=CARTESIAN_POINT('Ctrl Pts',(-50.4784766249808,-5.91664036532686,
-0.916335962829449));
#27747=CARTESIAN_POINT('Ctrl Pts',(-50.4353280577568,-5.7003400533041,-1.83299539734153));
#27748=CARTESIAN_POINT('Ctrl Pts',(-50.3921794905327,-5.28961211713201,
-2.65217033476586));
#27749=CARTESIAN_POINT('Ctrl Pts',(-50.3457599425051,-4.84774796297761,
-3.53344479640325));
#27750=CARTESIAN_POINT('Ctrl Pts',(-50.2993403944775,-4.18086074900938,
-4.30189444770271));
#27751=CARTESIAN_POINT('Ctrl Pts',(-50.2529208464499,-3.37058688269006,
-4.86345020541586));
#27752=CARTESIAN_POINT('Ctrl Pts',(-50.2065012984223,-2.56031301637074,
-5.425005963129));
#27753=CARTESIAN_POINT('Ctrl Pts',(-50.1600817503947,-1.60665249770033,
-5.77966782725582));
#27754=CARTESIAN_POINT('Ctrl Pts',(-50.113662202367,-0.626346834167139,
-5.88402017991531));
#27755=CARTESIAN_POINT('Ctrl Pts',(-50.0672426543394,0.35395882936604,-5.98837253257481));
#27756=CARTESIAN_POINT('Ctrl Pts',(-50.0208231063118,1.36090963776204,-5.842415373767));
#27757=CARTESIAN_POINT('Ctrl Pts',(-49.9744035582842,2.27124059992882,-5.4640159197752));
#27758=CARTESIAN_POINT('Ctrl Pts',(-49.9279840102566,3.18157156209561,-5.08561646578339));
#27759=CARTESIAN_POINT('Ctrl Pts',(-49.881564462229,3.9952826780332,-4.47477471660759));
#27760=CARTESIAN_POINT('Ctrl Pts',(-49.8351449142014,4.61276422239933,-3.70626632379198));
#27761=CARTESIAN_POINT('Ctrl Pts',(-49.7887253661737,5.23024576676547,-2.93775793097636));
#27762=CARTESIAN_POINT('Ctrl Pts',(-49.7423058181462,5.65149773956015,-2.01158289452093));
#27763=CARTESIAN_POINT('Ctrl Pts',(-49.6958862701186,5.82495295374594,-1.04111811095968));
#27764=CARTESIAN_POINT('Ctrl Pts',(-49.6494667220909,5.99840816793174,-0.0706533273984164));
#27765=CARTESIAN_POINT('Ctrl Pts',(-49.6030471740633,5.92406662350867,0.944101203268662));
#27766=CARTESIAN_POINT('Ctrl Pts',(-49.5566276260357,5.61102877477366,1.87892520420157));
#27767=CARTESIAN_POINT('Ctrl Pts',(-49.5102080780081,5.29799092603865,2.81374920513445));
#27768=CARTESIAN_POINT('Ctrl Pts',(-49.4637885299805,4.74625677299171,3.66864267633316));
#27769=CARTESIAN_POINT('Ctrl Pts',(-49.4173689819529,4.0233663631639,4.33895459092201));
#27770=CARTESIAN_POINT('Ctrl Pts',(-49.3709494339252,3.30047595333607,5.00926650551086));
#27771=CARTESIAN_POINT('Ctrl Pts',(-49.3245298858977,2.40642928672737,5.49499686348987));
#27772=CARTESIAN_POINT('Ctrl Pts',(-49.27811033787,1.45067029394137,5.73668541342454));
#27773=CARTESIAN_POINT('Ctrl Pts',(-49.2316907898424,0.494911301155378,
5.97837396335922));
#27774=CARTESIAN_POINT('Ctrl Pts',(-49.1852712418148,-0.522560017807911,
5.97602070524955));
#27775=CARTESIAN_POINT('Ctrl Pts',(-49.1388516937872,-1.47719081287612,
5.72991371110214));
#27776=CARTESIAN_POINT('Ctrl Pts',(-49.0924321457596,-2.43182160794432,
5.48380671695473));
#27777=CARTESIAN_POINT('Ctrl Pts',(-49.046012597732,-3.32361187911748,4.99394598676957));
#27778=CARTESIAN_POINT('Ctrl Pts',(-48.9995930497044,-4.0433939104401,4.32029738783544));
#27779=CARTESIAN_POINT('Ctrl Pts',(-48.9531735016768,-4.76317594176271,
3.64664878890133));
#27780=CARTESIAN_POINT('Ctrl Pts',(-48.9067539536491,-5.3109497332348,2.78921232121828));
#27781=CARTESIAN_POINT('Ctrl Pts',(-48.8603344056215,-5.61966004147882,
1.85295031032353));
#27782=CARTESIAN_POINT('Ctrl Pts',(-48.8307646678159,-5.81631173802741,
1.2565416127853));
#27783=CARTESIAN_POINT('Ctrl Pts',(-48.8011949300104,-5.91595569718159,
0.628146902608916));
#27784=CARTESIAN_POINT('Ctrl Pts',(-48.7716251922048,-5.91638811723421,
-0.000113882446527966));
#27785=CARTESIAN_POINT('Origin',(-29.75,0.,0.));
#27786=CARTESIAN_POINT('',(-46.7698748077951,-5.91699642112564,0.00013125821292051));
#27787=CARTESIAN_POINT('',(-47.0216251922048,-5.91683542453774,0.000151426803681578));
#27788=CARTESIAN_POINT('',(-29.75,-5.91675,-7.2459289488551E-16));
#27789=CARTESIAN_POINT('Ctrl Pts',(-46.7698748077951,-5.91699642112564,
0.00013125821292051));
#27790=CARTESIAN_POINT('Ctrl Pts',(-46.7768846758079,-5.91714010263027,
0.149024142477122));
#27791=CARTESIAN_POINT('Ctrl Pts',(-46.7838945438206,-5.91163420665211,
0.297906424512786));
#27792=CARTESIAN_POINT('Ctrl Pts',(-46.7909044118334,-5.90040426837894,
0.446355692343765));
#27793=CARTESIAN_POINT('Ctrl Pts',(-46.837323959861,-5.826039293451,1.42939102270706));
#27794=CARTESIAN_POINT('Ctrl Pts',(-46.8837435078887,-5.5006678187631,2.39343813211343));
#27795=CARTESIAN_POINT('Ctrl Pts',(-46.9301630559163,-4.96411990512314,
3.22048404777175));
#27796=CARTESIAN_POINT('Ctrl Pts',(-46.9765826039439,-4.42757199148317,
4.04752996343008));
#27797=CARTESIAN_POINT('Ctrl Pts',(-47.0230021519715,-3.67984763889115,
4.73757468534036));
#27798=CARTESIAN_POINT('Ctrl Pts',(-47.0694216999991,-2.81247886151601,
5.20614700022172));
#27799=CARTESIAN_POINT('Ctrl Pts',(-47.1158412480267,-1.9451100841409,5.67471931510307));
#27800=CARTESIAN_POINT('Ctrl Pts',(-47.1622607960543,-0.958096881982646,
5.92181922295553));
#27801=CARTESIAN_POINT('Ctrl Pts',(-47.2086803440819,0.0277363982703663,
5.91719820747988));
#27802=CARTESIAN_POINT('Ctrl Pts',(-47.2550998921095,1.01356967852341,5.91257719200423));
#27803=CARTESIAN_POINT('Ctrl Pts',(-47.3015194401372,1.99822303687121,5.65623525320047));
#27804=CARTESIAN_POINT('Ctrl Pts',(-47.3479389881648,2.86116100481487,5.17955226239864));
#27805=CARTESIAN_POINT('Ctrl Pts',(-47.3943585361924,3.72409897275852,4.70286927159681));
#27806=CARTESIAN_POINT('Ctrl Pts',(-47.44077808422,4.46532155029799,4.00584522879691));
#27807=CARTESIAN_POINT('Ctrl Pts',(-47.4871976322476,4.99409263229707,3.17380571466311));
#27808=CARTESIAN_POINT('Ctrl Pts',(-47.5336171802752,5.52286371429616,2.3417662005293));
#27809=CARTESIAN_POINT('Ctrl Pts',(-47.5800367283028,5.83918330075486,1.37471121506159));
#27810=CARTESIAN_POINT('Ctrl Pts',(-47.6264562763305,5.90432940974324,0.391021937534293));
#27811=CARTESIAN_POINT('Ctrl Pts',(-47.6728758243581,5.96947551873162,-0.592667339993006));
#27812=CARTESIAN_POINT('Ctrl Pts',(-47.7192953723857,5.78344815024968,-1.59299090957989));
#27813=CARTESIAN_POINT('Ctrl Pts',(-47.7657149204133,5.36901967979738,-2.48749504770171));
#27814=CARTESIAN_POINT('Ctrl Pts',(-47.8121344684409,4.95459120934508,-3.38199918582354));
#27815=CARTESIAN_POINT('Ctrl Pts',(-47.8585540164685,4.31176163692242,-4.1706838924803));
#27816=CARTESIAN_POINT('Ctrl Pts',(-47.9049735644961,3.51922237511646,-4.75700302804946));
#27817=CARTESIAN_POINT('Ctrl Pts',(-47.9513931125237,2.7266831133105,-5.34332216361862));
#27818=CARTESIAN_POINT('Ctrl Pts',(-47.9978126605514,1.78443416212123,-5.72727572810017));
#27819=CARTESIAN_POINT('Ctrl Pts',(-48.044232208579,0.807820092113927,-5.86186238606547));
#27820=CARTESIAN_POINT('Ctrl Pts',(-48.0906517566066,-0.168793977893349,
-5.99644904403077));
#27821=CARTESIAN_POINT('Ctrl Pts',(-48.1370713046342,-1.17977316671866,
-5.88166879547983));
#27822=CARTESIAN_POINT('Ctrl Pts',(-48.1834908526618,-2.10135935264875,
-5.53157236284835));
#27823=CARTESIAN_POINT('Ctrl Pts',(-48.2299104006894,-3.02294553857886,
-5.18147593021687));
#27824=CARTESIAN_POINT('Ctrl Pts',(-48.2763299487171,-3.85513872161374,
-4.59606331350482));
#27825=CARTESIAN_POINT('Ctrl Pts',(-48.3227494967447,-4.49606671054176,
-3.84699727953507));
#27826=CARTESIAN_POINT('Ctrl Pts',(-48.3691690447723,-5.13699469946979,
-3.09793124556532));
#27827=CARTESIAN_POINT('Ctrl Pts',(-48.4155885927998,-5.58665749429096,
-2.18521179433785));
#27828=CARTESIAN_POINT('Ctrl Pts',(-48.4620081408275,-5.79001002236034,
-1.22056866884206));
#27829=CARTESIAN_POINT('Ctrl Pts',(-48.4812970298167,-5.87450986146415,
-0.819726890916495));
#27830=CARTESIAN_POINT('Ctrl Pts',(-48.5005859188059,-5.91647972563172,
-0.40991954044558));
#27831=CARTESIAN_POINT('Ctrl Pts',(-48.5198748077951,-5.91629691922315,
-7.52784257820882E-5));
#27832=CARTESIAN_POINT('Ctrl Pts',(-48.7716251922048,-5.91638811723421,
-0.000113882446527966));
#27833=CARTESIAN_POINT('Ctrl Pts',(-48.7547753819828,-5.91663452441816,
-0.358117564040023));
#27834=CARTESIAN_POINT('Ctrl Pts',(-48.7379255717607,-5.88466599601319,
-0.716077758865912));
#27835=CARTESIAN_POINT('Ctrl Pts',(-48.7210757615387,-5.82007476214659,
-1.06805130838649));
#27836=CARTESIAN_POINT('Ctrl Pts',(-48.6746562135111,-5.64213234955439,
-2.0377033620953));
#27837=CARTESIAN_POINT('Ctrl Pts',(-48.6282366654835,-5.21660069935406,
-2.96191991540646));
#27838=CARTESIAN_POINT('Ctrl Pts',(-48.5818171174559,-4.59557089150098,
-3.727563817765));
#27839=CARTESIAN_POINT('Ctrl Pts',(-48.5353975694282,-3.9745410836479,-4.49320772012353));
#27840=CARTESIAN_POINT('Ctrl Pts',(-48.4889780214006,-3.15801311814206,
-5.10027897152943));
#27841=CARTESIAN_POINT('Ctrl Pts',(-48.442558473373,-2.24594154247006,-5.47446348258247));
#27842=CARTESIAN_POINT('Ctrl Pts',(-48.3961389253454,-1.33386996679804,
-5.84864799363553));
#27843=CARTESIAN_POINT('Ctrl Pts',(-48.3497193773178,-0.326254780959847,
-5.98994576433573));
#27844=CARTESIAN_POINT('Ctrl Pts',(-48.3032998292902,0.653557694776576,
-5.88105995326694));
#27845=CARTESIAN_POINT('Ctrl Pts',(-48.2568802812626,1.63337017051296,-5.77217414219816));
#27846=CARTESIAN_POINT('Ctrl Pts',(-48.2104607332349,2.58537993614758,-5.4131047493604));
#27847=CARTESIAN_POINT('Ctrl Pts',(-48.1640411852073,3.3930475596625,-4.84780693635691));
#27848=CARTESIAN_POINT('Ctrl Pts',(-48.1176216371797,4.20071518317745,-4.28250912335339));
#27849=CARTESIAN_POINT('Ctrl Pts',(-48.0712020891521,4.86404066457271,-3.51098289018414));
#27850=CARTESIAN_POINT('Ctrl Pts',(-48.0247825411245,5.3018236027229,-2.62767393714141));
#27851=CARTESIAN_POINT('Ctrl Pts',(-47.9783629930969,5.73960654087308,-1.74436498409869));
#27852=CARTESIAN_POINT('Ctrl Pts',(-47.9319434450693,5.95184693577819,-0.749273311182518));
#27853=CARTESIAN_POINT('Ctrl Pts',(-47.8855238970416,5.91256356753235,0.235787816078176));
#27854=CARTESIAN_POINT('Ctrl Pts',(-47.839104349014,5.87328019928651,1.22084894333886));
#27855=CARTESIAN_POINT('Ctrl Pts',(-47.7926848009865,5.58247306788974,2.19587952494403));
#27856=CARTESIAN_POINT('Ctrl Pts',(-47.7462652529588,5.07574107068855,3.0415220560843));
#27857=CARTESIAN_POINT('Ctrl Pts',(-47.6998457049312,4.56900907348736,3.88716458722458));
#27858=CARTESIAN_POINT('Ctrl Pts',(-47.6534261569035,3.84635221048174,4.60341906789995));
#27859=CARTESIAN_POINT('Ctrl Pts',(-47.6070066088759,2.99623388131174,5.10260584043109));
#27860=CARTESIAN_POINT('Ctrl Pts',(-47.5605870608483,2.14611555214175,5.60179261296221));
#27861=CARTESIAN_POINT('Ctrl Pts',(-47.5141675128208,1.16853575680737,5.88391167734911));
#27862=CARTESIAN_POINT('Ctrl Pts',(-47.4677479647932,0.183164059858164,
5.914427678271));
#27863=CARTESIAN_POINT('Ctrl Pts',(-47.4213284167656,-0.802207637091027,
5.94494367919289));
#27864=CARTESIAN_POINT('Ctrl Pts',(-47.3749088687379,-1.79537123565506,
5.72385661664975));
#27865=CARTESIAN_POINT('Ctrl Pts',(-47.3284893207102,-2.67474949381855,
5.27823066752859));
#27866=CARTESIAN_POINT('Ctrl Pts',(-47.2820697726826,-3.55412775198207,
4.83260471840741));
#27867=CARTESIAN_POINT('Ctrl Pts',(-47.2356502246551,-4.31972066974506,
4.16243988270822));
#27868=CARTESIAN_POINT('Ctrl Pts',(-47.1892306766275,-4.87780886836403,
3.34977379505408));
#27869=CARTESIAN_POINT('Ctrl Pts',(-47.1428111285999,-5.43589706698301,
2.53710770739995));
#27870=CARTESIAN_POINT('Ctrl Pts',(-47.0963915805722,-5.78648054645795,
1.5819403677909));
#27871=CARTESIAN_POINT('Ctrl Pts',(-47.0499720325446,-5.88664294075176,
0.601197739865422));
#27872=CARTESIAN_POINT('Ctrl Pts',(-47.0405230857647,-5.90703153075849,
0.401562342929505));
#27873=CARTESIAN_POINT('Ctrl Pts',(-47.0310741389847,-5.91704397930712,
0.200867239662508));
#27874=CARTESIAN_POINT('Ctrl Pts',(-47.0216251922048,-5.91683542453774,
0.000151426803681578));
#27875=CARTESIAN_POINT('Origin',(-29.75,0.,0.));
#27876=CARTESIAN_POINT('',(-45.0198748077951,-5.91659248732073,-0.000150399349319874));
#27877=CARTESIAN_POINT('',(-45.2716251922049,-5.91675241673656,-0.000155248934938149));
#27878=CARTESIAN_POINT('',(-29.75,-5.91675,-7.2459289488551E-16));
#27879=CARTESIAN_POINT('Ctrl Pts',(-45.0198748077951,-5.91659248732073,
-0.000150399349319874));
#27880=CARTESIAN_POINT('Ctrl Pts',(-45.0531834328098,-5.91591598728341,
0.707479493305166));
#27881=CARTESIAN_POINT('Ctrl Pts',(-45.0864920578246,-5.78888701238488,
1.41534572504519));
#27882=CARTESIAN_POINT('Ctrl Pts',(-45.1198006828394,-5.54050131005888,
2.07770285835773));
#27883=CARTESIAN_POINT('Ctrl Pts',(-45.166220230867,-5.1943461615535,3.00077664923348));
#27884=CARTESIAN_POINT('Ctrl Pts',(-45.2126397788946,-4.61249498655612,
3.83546379772058));
#27885=CARTESIAN_POINT('Ctrl Pts',(-45.2590593269222,-3.86617458115737,
4.47958681603613));
#27886=CARTESIAN_POINT('Ctrl Pts',(-45.3054788749499,-3.11985417575861,
5.12370983435168));
#27887=CARTESIAN_POINT('Ctrl Pts',(-45.3518984229774,-2.20906453995847,
5.57726872249568));
#27888=CARTESIAN_POINT('Ctrl Pts',(-45.398317971005,-1.24529918010056,5.78474147101086));
#27889=CARTESIAN_POINT('Ctrl Pts',(-45.4447375190326,-0.281533820242672,
5.99221421952604));
#27890=CARTESIAN_POINT('Ctrl Pts',(-45.4911570670603,0.735207263672997,
5.95360082841241));
#27891=CARTESIAN_POINT('Ctrl Pts',(-45.5375766150879,1.6804606126505,5.67362812173325));
#27892=CARTESIAN_POINT('Ctrl Pts',(-45.5839961631155,2.62571396162803,5.39365541505408));
#27893=CARTESIAN_POINT('Ctrl Pts',(-45.6304157111431,3.4994795756674,4.87232339280936));
#27894=CARTESIAN_POINT('Ctrl Pts',(-45.6768352591707,4.19479621124706,4.17345045262303));
#27895=CARTESIAN_POINT('Ctrl Pts',(-45.7232548071983,4.89011284682673,3.47457751243669));
#27896=CARTESIAN_POINT('Ctrl Pts',(-45.769674355226,5.40698050394668,2.59816365430878));
#27897=CARTESIAN_POINT('Ctrl Pts',(-45.8160939032536,5.68212728628449,1.65149430421464));
#27898=CARTESIAN_POINT('Ctrl Pts',(-45.8625134512812,5.9572740686223,0.7048249541205));
#27899=CARTESIAN_POINT('Ctrl Pts',(-45.9089329993088,5.99069997617795,-0.312099887939838));
#27900=CARTESIAN_POINT('Ctrl Pts',(-45.9553525473364,5.77831320609204,-1.27479426837995));
#27901=CARTESIAN_POINT('Ctrl Pts',(-46.001772095364,5.56592643600614,-2.23748864882004));
#27902=CARTESIAN_POINT('Ctrl Pts',(-46.0481916433916,5.10772698827866,-3.14595256763994));
#27903=CARTESIAN_POINT('Ctrl Pts',(-46.0946111914192,4.45980494235696,-3.88897721907965));
#27904=CARTESIAN_POINT('Ctrl Pts',(-46.1410307394469,3.81188289643525,-4.63200187051937));
#27905=CARTESIAN_POINT('Ctrl Pts',(-46.1874502874745,2.97423825231934,-5.2095872545789));
#27906=CARTESIAN_POINT('Ctrl Pts',(-46.2338698355021,2.04941053699924,-5.551028768186));
#27907=CARTESIAN_POINT('Ctrl Pts',(-46.2802893835297,1.12458282167914,-5.89247028179309));
#27908=CARTESIAN_POINT('Ctrl Pts',(-46.3267089315573,0.112572035154879,
-5.99776792494772));
#27909=CARTESIAN_POINT('Ctrl Pts',(-46.3731284795849,-0.8627374187419,-5.85403177995257));
#27910=CARTESIAN_POINT('Ctrl Pts',(-46.4195480276125,-1.83804687263868,
-5.71029563495742));
#27911=CARTESIAN_POINT('Ctrl Pts',(-46.4659675756401,-2.77665499390798,
-5.31752570181249));
#27912=CARTESIAN_POINT('Ctrl Pts',(-46.5123871236677,-3.56366290095356,
-4.72380256390541));
#27913=CARTESIAN_POINT('Ctrl Pts',(-46.5588066716953,-4.35067080799912,
-4.13007942599834));
#27914=CARTESIAN_POINT('Ctrl Pts',(-46.605226219723,-4.98607850082097,-3.33540308332912));
#27915=CARTESIAN_POINT('Ctrl Pts',(-46.6516457677506,-5.3921031096479,-2.43705313633443));
#27916=CARTESIAN_POINT('Ctrl Pts',(-46.6910554477654,-5.73681348689026,
-1.67436402244332));
#27917=CARTESIAN_POINT('Ctrl Pts',(-46.7304651277802,-5.91618863956524,
-0.836948828693407));
#27918=CARTESIAN_POINT('Ctrl Pts',(-46.7698748077951,-5.91699642112564,
0.00013125821292051));
#27919=CARTESIAN_POINT('Ctrl Pts',(-47.0216251922048,-5.91683542453774,
0.000151426803681578));
#27920=CARTESIAN_POINT('Ctrl Pts',(-46.9846545909571,-5.91601941875459,
-0.785183114085889));
#27921=CARTESIAN_POINT('Ctrl Pts',(-46.9476839897095,-5.75873029000744,
-1.5708346976774));
#27922=CARTESIAN_POINT('Ctrl Pts',(-46.9107133884618,-5.45426065261164,
-2.2945684927006));
#27923=CARTESIAN_POINT('Ctrl Pts',(-46.8642938404342,-5.07197466106503,
-3.20327418109923));
#27924=CARTESIAN_POINT('Ctrl Pts',(-46.8178742924066,-4.45766136885915,
-4.01436764165459));
#27925=CARTESIAN_POINT('Ctrl Pts',(-46.7714547443789,-3.68652139340255,
-4.62855958698894));
#27926=CARTESIAN_POINT('Ctrl Pts',(-46.7250351963513,-2.91538141794593,
-5.24275153232329));
#27927=CARTESIAN_POINT('Ctrl Pts',(-46.6786156483237,-1.98741475923859,
-5.66004196243661));
#27928=CARTESIAN_POINT('Ctrl Pts',(-46.6321961002961,-1.01621763366518,
-5.82934863902905));
#27929=CARTESIAN_POINT('Ctrl Pts',(-46.5857765522685,-0.045020508091773,
-5.99865531562148));
#27930=CARTESIAN_POINT('Ctrl Pts',(-46.5393570042409,0.969407084347734,
-5.91997823869303));
#27931=CARTESIAN_POINT('Ctrl Pts',(-46.4929374562133,1.90288488866676,-5.60294859291119));
#27932=CARTESIAN_POINT('Ctrl Pts',(-46.4465179081857,2.83636269298577,-5.28591894712936));
#27933=CARTESIAN_POINT('Ctrl Pts',(-46.4000983601581,3.6888907091843,-4.73053673249415));
#27934=CARTESIAN_POINT('Ctrl Pts',(-46.3536788121304,4.35610747546488,-4.00478857076387));
#27935=CARTESIAN_POINT('Ctrl Pts',(-46.3072592641028,5.02332424174547,-3.27904040903357));
#27936=CARTESIAN_POINT('Ctrl Pts',(-46.2608397160752,5.50522975810808,-2.38292630020819));
#27937=CARTESIAN_POINT('Ctrl Pts',(-46.2144201680476,5.74283198771603,-1.42614325899866));
#27938=CARTESIAN_POINT('Ctrl Pts',(-46.16800062002,5.98043421732399,-0.469360217789129));
#27939=CARTESIAN_POINT('Ctrl Pts',(-46.1215810719924,5.97373316017729,0.548091755804578));
#27940=CARTESIAN_POINT('Ctrl Pts',(-46.0751615239648,5.72354912024968,1.50166217985638));
#27941=CARTESIAN_POINT('Ctrl Pts',(-46.0287419759371,5.47336508032206,2.45523260390819));
#27942=CARTESIAN_POINT('Ctrl Pts',(-45.9823224279095,4.97969805761354,3.34492147841808));
#27943=CARTESIAN_POINT('Ctrl Pts',(-45.9359028798819,4.3029798633399,4.06181832804142));
#27944=CARTESIAN_POINT('Ctrl Pts',(-45.8894833318543,3.62626166906627,4.77871517766474));
#27945=CARTESIAN_POINT('Ctrl Pts',(-45.8430637838267,2.76649230322752,5.3228200024015));
#27946=CARTESIAN_POINT('Ctrl Pts',(-45.7966442357991,1.82891967102184,5.62752669218647));
#27947=CARTESIAN_POINT('Ctrl Pts',(-45.7502246877715,0.891347038816158,
5.93223338197144));
#27948=CARTESIAN_POINT('Ctrl Pts',(-45.7038051397438,-0.12402885975648,
5.99754193680463));
#27949=CARTESIAN_POINT('Ctrl Pts',(-45.6573855917162,-1.09291168365437,
5.81545766780686));
#27950=CARTESIAN_POINT('Ctrl Pts',(-45.6109660436886,-2.06179450755229,
5.63337339880909));
#27951=CARTESIAN_POINT('Ctrl Pts',(-45.564546495661,-2.98418425677548,5.20389630598036));
#27952=CARTESIAN_POINT('Ctrl Pts',(-45.5181269476334,-3.74716740737289,
4.57960044713992));
#27953=CARTESIAN_POINT('Ctrl Pts',(-45.4717073996058,-4.51015055797028,
3.95530458829949));
#27954=CARTESIAN_POINT('Ctrl Pts',(-45.4252878515782,-5.11372710994189,
3.13618996344739));
#27955=CARTESIAN_POINT('Ctrl Pts',(-45.3788683035506,-5.4840107744226,2.22252776368231));
#27956=CARTESIAN_POINT('Ctrl Pts',(-45.3431205997687,-5.76916630297845,
1.51891630985034));
#27957=CARTESIAN_POINT('Ctrl Pts',(-45.3073728959868,-5.91596647289002,
0.759233006693162));
#27958=CARTESIAN_POINT('Ctrl Pts',(-45.2716251922049,-5.91675241673656,
-0.000155248934938149));
#27959=CARTESIAN_POINT('Origin',(-29.75,0.,0.));
#27960=CARTESIAN_POINT('',(-43.2698748077951,-5.91658768614795,0.000149985469924119));
#27961=CARTESIAN_POINT('',(-43.5216251922048,-5.9164475069627,0.000129275767947919));
#27962=CARTESIAN_POINT('',(-29.75,-5.91675,-7.2459289488551E-16));
#27963=CARTESIAN_POINT('Ctrl Pts',(-43.2698748077951,-5.91658768614795,
0.000149985469924119));
#27964=CARTESIAN_POINT('Ctrl Pts',(-43.2830626417842,-5.91685444793391,
0.280321481177761));
#27965=CARTESIAN_POINT('Ctrl Pts',(-43.2962504757734,-5.89731610636416,
0.560456079724737));
#27966=CARTESIAN_POINT('Ctrl Pts',(-43.3094383097625,-5.85766495001964,
0.837714311506925));
#27967=CARTESIAN_POINT('Ctrl Pts',(-43.3558578577901,-5.71809777334743,
1.81362906876509));
#27968=CARTESIAN_POINT('Ctrl Pts',(-43.4022774058177,-5.32934225143748,
2.75390699038182));
#27969=CARTESIAN_POINT('Ctrl Pts',(-43.4486969538453,-4.73898754708268,
3.54344478763073));
#27970=CARTESIAN_POINT('Ctrl Pts',(-43.4951165018729,-4.14863284272788,
4.33298258487964));
#27971=CARTESIAN_POINT('Ctrl Pts',(-43.5415360499005,-3.35667895592823,
4.97178025776071));
#27972=CARTESIAN_POINT('Ctrl Pts',(-43.5879555979282,-2.4600722200971,5.3816399550972));
#27973=CARTESIAN_POINT('Ctrl Pts',(-43.6343751459558,-1.563465484266,5.79149965243368));
#27974=CARTESIAN_POINT('Ctrl Pts',(-43.6807946939834,-0.56220589940344,
5.97242137422558));
#27975=CARTESIAN_POINT('Ctrl Pts',(-43.727214242011,0.421138229485253,5.90225774818909));
#27976=CARTESIAN_POINT('Ctrl Pts',(-43.7736337900386,1.40448235837399,5.8320941221526));
#27977=CARTESIAN_POINT('Ctrl Pts',(-43.8200533380662,2.36991103128888,5.51084514828768));
#27978=CARTESIAN_POINT('Ctrl Pts',(-43.8664728860938,3.19924215256585,4.97783623511641));
#27979=CARTESIAN_POINT('Ctrl Pts',(-43.9128924341214,4.02857327384278,4.44482732194516));
#27980=CARTESIAN_POINT('Ctrl Pts',(-43.9593119821491,4.72180684348183,3.70005846946757));
#27981=CARTESIAN_POINT('Ctrl Pts',(-44.0057315301767,5.19408128823263,2.8346998969245));
#27982=CARTESIAN_POINT('Ctrl Pts',(-44.0521510782043,5.66635573298344,1.9693413243814));
#27983=CARTESIAN_POINT('Ctrl Pts',(-44.0985706262319,5.91767105284598,0.98339303177284));
#27984=CARTESIAN_POINT('Ctrl Pts',(-44.1449901742595,5.91726270559451,-0.00245099417194854));
#27985=CARTESIAN_POINT('Ctrl Pts',(-44.1914097222871,5.91685435834304,-0.988295020116738));
#27986=CARTESIAN_POINT('Ctrl Pts',(-44.2378292703147,5.66472234397756,-1.97403477939774));
#27987=CARTESIAN_POINT('Ctrl Pts',(-44.2842488183423,5.19173117965784,-2.83900181270824));
#27988=CARTESIAN_POINT('Ctrl Pts',(-44.3306683663699,4.71874001533813,-3.70396884601872));
#27989=CARTESIAN_POINT('Ctrl Pts',(-44.3770879143976,4.02488970106418,-4.4481631533587));
#27990=CARTESIAN_POINT('Ctrl Pts',(-44.4235074624252,3.19511730833444,-4.98048484792131));
#27991=CARTESIAN_POINT('Ctrl Pts',(-44.4699270104528,2.36534491560469,-5.51280654248393));
#27992=CARTESIAN_POINT('Ctrl Pts',(-44.5163465584804,1.3996504444191,-5.83325562426917));
#27993=CARTESIAN_POINT('Ctrl Pts',(-44.562766106508,0.416248527901588,-5.90260460283525));
#27994=CARTESIAN_POINT('Ctrl Pts',(-44.6091856545356,-0.567153388615943,
-5.97195358140132));
#27995=CARTESIAN_POINT('Ctrl Pts',(-44.6556052025633,-1.56826275046543,
-5.79020245674823));
#27996=CARTESIAN_POINT('Ctrl Pts',(-44.7020247505909,-2.4645296420586,-5.37960013177621));
#27997=CARTESIAN_POINT('Ctrl Pts',(-44.7484442986185,-3.36079653365177,
-4.96899780680419));
#27998=CARTESIAN_POINT('Ctrl Pts',(-44.7948638466461,-4.1522209549886,-4.32954428151325));
#27999=CARTESIAN_POINT('Ctrl Pts',(-44.8412833946737,-4.74192138670128,
-3.53951769267185));
#28000=CARTESIAN_POINT('Ctrl Pts',(-44.8877029427013,-5.33162181841396,
-2.74949110383044));
#28001=CARTESIAN_POINT('Ctrl Pts',(-44.9341224907289,-5.71959826050248,
-1.80889145143859));
#28002=CARTESIAN_POINT('Ctrl Pts',(-44.9805420387565,-5.85835692054005,
-0.832861408610456));
#28003=CARTESIAN_POINT('Ctrl Pts',(-44.9936529617694,-5.89754847208288,
-0.557187575204382));
#28004=CARTESIAN_POINT('Ctrl Pts',(-45.0067638847822,-5.91685877090054,
-0.278687296026193));
#28005=CARTESIAN_POINT('Ctrl Pts',(-45.0198748077951,-5.91659248732073,
-0.000150399349319874));
#28006=CARTESIAN_POINT('Ctrl Pts',(-45.2716251922049,-5.91675241673656,
-0.000155248934938149));
#28007=CARTESIAN_POINT('Ctrl Pts',(-45.2609533479592,-5.91698704636109,
-0.226857171819796));
#28008=CARTESIAN_POINT('Ctrl Pts',(-45.2502815037135,-5.90420866411302,
-0.453532799616136));
#28009=CARTESIAN_POINT('Ctrl Pts',(-45.2396096594678,-5.87821350079514,
-0.678682454017764));
#28010=CARTESIAN_POINT('Ctrl Pts',(-45.1931901114401,-5.76514178569715,
-1.65802069727473));
#28011=CARTESIAN_POINT('Ctrl Pts',(-45.1467705634125,-5.40200757851135,
-2.60848740911062));
#28012=CARTESIAN_POINT('Ctrl Pts',(-45.1003510153849,-4.83326363148813,
-3.41373204907123));
#28013=CARTESIAN_POINT('Ctrl Pts',(-45.0539314673573,-4.26451968446491,
-4.21897668903183));
#28014=CARTESIAN_POINT('Ctrl Pts',(-45.0075119193297,-3.49016599760425,
-4.87899925711716));
#28015=CARTESIAN_POINT('Ctrl Pts',(-44.9610923713021,-2.60499439143712,
-5.31300367540839));
#28016=CARTESIAN_POINT('Ctrl Pts',(-44.9146728232745,-1.71982278526999,
-5.74700809369961));
#28017=CARTESIAN_POINT('Ctrl Pts',(-44.8682532752468,-0.723833259796379,
-5.95499436219676));
#28018=CARTESIAN_POINT('Ctrl Pts',(-44.8218337272192,0.261051009629444,
-5.91150202610921));
#28019=CARTESIAN_POINT('Ctrl Pts',(-44.7754141791916,1.2459352790553,-5.86800969002166));
#28020=CARTESIAN_POINT('Ctrl Pts',(-44.728994631164,2.21971429243333,-5.57303874934939));
#28021=CARTESIAN_POINT('Ctrl Pts',(-44.6825750831364,3.06318375456983,-5.06269781046245));
#28022=CARTESIAN_POINT('Ctrl Pts',(-44.6361555351088,3.90665321670632,-4.55235687157551));
#28023=CARTESIAN_POINT('Ctrl Pts',(-44.5897359870811,4.61981312760129,-3.82664593447388));
#28024=CARTESIAN_POINT('Ctrl Pts',(-44.5433164390535,5.11536264859339,-2.97440226057227));
#28025=CARTESIAN_POINT('Ctrl Pts',(-44.4968968910259,5.6109121695855,-2.12215858667066));
#28026=CARTESIAN_POINT('Ctrl Pts',(-44.4504773429983,5.88885130067477,-1.14338217596907));
#28027=CARTESIAN_POINT('Ctrl Pts',(-44.4040577949707,5.91515636937177,-0.157889075627079));
#28028=CARTESIAN_POINT('Ctrl Pts',(-44.3576382469431,5.94146143806878,0.827604024714909));
#28029=CARTESIAN_POINT('Ctrl Pts',(-44.3112186989155,5.71613244437352,1.81981381469727));
#28030=CARTESIAN_POINT('Ctrl Pts',(-44.2647991508879,5.2667528374168,2.69727981193718));
#28031=CARTESIAN_POINT('Ctrl Pts',(-44.2183796028602,4.81737323046008,3.5747458091771));
#28032=CARTESIAN_POINT('Ctrl Pts',(-44.1719600548327,4.14394301024188,4.33746801367458));
#28033=CARTESIAN_POINT('Ctrl Pts',(-44.1255405068051,3.32889954053823,4.89207846250714));
#28034=CARTESIAN_POINT('Ctrl Pts',(-44.0791209587774,2.51385607083456,5.44668891133971));
#28035=CARTESIAN_POINT('Ctrl Pts',(-44.0327014107498,1.55719935164544,5.79318760450736));
#28036=CARTESIAN_POINT('Ctrl Pts',(-43.9862818627222,0.576037667691109,
5.88915821146986));
#28037=CARTESIAN_POINT('Ctrl Pts',(-43.9398623146946,-0.405124016263193,
5.98512881843235));
#28038=CARTESIAN_POINT('Ctrl Pts',(-43.893442766667,-1.41079066498267,5.8305713391897));
#28039=CARTESIAN_POINT('Ctrl Pts',(-43.8470232186394,-2.31785448664446,
5.4444057906317));
#28040=CARTESIAN_POINT('Ctrl Pts',(-43.8006036706118,-3.22491830830626,
5.05824024207369));
#28041=CARTESIAN_POINT('Ctrl Pts',(-43.7541841225842,-4.03337930291038,
4.44046662420031));
#28042=CARTESIAN_POINT('Ctrl Pts',(-43.7077645745565,-4.64427043406613,
3.66670914712104));
#28043=CARTESIAN_POINT('Ctrl Pts',(-43.6613450265289,-5.2551615652219,2.89295167004174));
#28044=CARTESIAN_POINT('Ctrl Pts',(-43.6149254785013,-5.66848283292931,
1.96321033375654));
#28045=CARTESIAN_POINT('Ctrl Pts',(-43.5685059304737,-5.83363788038793,
0.99129860023346));
#28046=CARTESIAN_POINT('Ctrl Pts',(-43.5528790177174,-5.8892365156086,0.664109290730965));
#28047=CARTESIAN_POINT('Ctrl Pts',(-43.5372521049611,-5.91671049438226,
0.332140813727917));
#28048=CARTESIAN_POINT('Ctrl Pts',(-43.5216251922048,-5.9164475069627,0.000129275767947919));
#28049=CARTESIAN_POINT('Origin',(-29.75,0.,0.));
#28050=CARTESIAN_POINT('',(-41.5198748077951,-5.91700124842561,-0.000130358588716351));
#28051=CARTESIAN_POINT('',(-41.7716251922048,-5.91713952097907,-9.42380742528296E-5));
#28052=CARTESIAN_POINT('',(-29.75,-5.91675,-7.2459289488551E-16));
#28053=CARTESIAN_POINT('Ctrl Pts',(-41.5198748077951,-5.91700124842561,
-0.000130358588716351));
#28054=CARTESIAN_POINT('Ctrl Pts',(-41.5593613987862,-5.91619546953019,
0.838581376832566));
#28055=CARTESIAN_POINT('Ctrl Pts',(-41.5988479897773,-5.73609840048565,
1.67762805962007));
#28056=CARTESIAN_POINT('Ctrl Pts',(-41.6383345807684,-5.39008235223998,
2.4415192340965));
#28057=CARTESIAN_POINT('Ctrl Pts',(-41.684754128796,-4.98331367034798,3.33953251332482));
#28058=CARTESIAN_POINT('Ctrl Pts',(-41.7311736768237,-4.3472478686121,4.13368219792937));
#28059=CARTESIAN_POINT('Ctrl Pts',(-41.7775932248513,-3.55974837862319,
4.72675315785388));
#28060=CARTESIAN_POINT('Ctrl Pts',(-41.8240127728789,-2.77224888863434,
5.31982411777835));
#28061=CARTESIAN_POINT('Ctrl Pts',(-41.8704323209065,-1.83331571039248,
5.7118163530228));
#28062=CARTESIAN_POINT('Ctrl Pts',(-41.9168518689341,-0.857887517055163,
5.85474448139908));
#28063=CARTESIAN_POINT('Ctrl Pts',(-41.9632714169617,0.11754067628218,5.99767260977537));
#28064=CARTESIAN_POINT('Ctrl Pts',(-42.0096909649893,1.12946388471498,5.89153663128348));
#28065=CARTESIAN_POINT('Ctrl Pts',(-42.0561105130169,2.05400842520608,5.54932908769831));
#28066=CARTESIAN_POINT('Ctrl Pts',(-42.1025300610446,2.97855296569718,5.20712154411313));
#28067=CARTESIAN_POINT('Ctrl Pts',(-42.1489496090722,3.81571883824659,4.62884243543466));
#28068=CARTESIAN_POINT('Ctrl Pts',(-42.1953691570998,4.46302512426135,3.88528128641982));
#28069=CARTESIAN_POINT('Ctrl Pts',(-42.2417887051274,5.11033141027611,3.14172013740498));
#28070=CARTESIAN_POINT('Ctrl Pts',(-42.288208253155,5.56777810975624,2.23287694805376));
#28071=CARTESIAN_POINT('Ctrl Pts',(-42.3346278011826,5.77936729026419,1.27000695219218));
#28072=CARTESIAN_POINT('Ctrl Pts',(-42.3810473492102,5.99095647077213,0.307136956330597));
#28073=CARTESIAN_POINT('Ctrl Pts',(-42.4274668972378,5.95668813230791,-0.709759846041339));
#28074=CARTESIAN_POINT('Ctrl Pts',(-42.4738864452654,5.68075720316425,-1.65620093379082));
#28075=CARTESIAN_POINT('Ctrl Pts',(-42.5203059932931,5.40482627402059,-2.60264202154027));
#28076=CARTESIAN_POINT('Ctrl Pts',(-42.5667255413207,4.88723275419751,-3.47862739466726));
#28077=CARTESIAN_POINT('Ctrl Pts',(-42.6131450893483,4.19133739585716,-4.17692407980818));
#28078=CARTESIAN_POINT('Ctrl Pts',(-42.6595646373759,3.49544203751678,-4.87522076494912));
#28079=CARTESIAN_POINT('Ctrl Pts',(-42.7059841854035,2.62124484065913,-5.39582876210398));
#28080=CARTESIAN_POINT('Ctrl Pts',(-42.7524037334311,1.67575988063407,-5.67501830453871));
#28081=CARTESIAN_POINT('Ctrl Pts',(-42.7988232814587,0.730274920609009,
-5.95420784697344));
#28082=CARTESIAN_POINT('Ctrl Pts',(-42.8452428294864,-0.286497802583452,
-5.99197893468805));
#28083=CARTESIAN_POINT('Ctrl Pts',(-42.891662377514,-1.25009095685333,-5.78370785344363));
#28084=CARTESIAN_POINT('Ctrl Pts',(-42.9380819255416,-2.21368411112319,
-5.57543677219922));
#28085=CARTESIAN_POINT('Ctrl Pts',(-42.9845014735692,-3.12409769647047,
-5.12112352199578));
#28086=CARTESIAN_POINT('Ctrl Pts',(-43.0309210215968,-3.8698842404346,-4.47638245685375));
#28087=CARTESIAN_POINT('Ctrl Pts',(-43.0773405696244,-4.61567078439876,
-3.8316413917117));
#28088=CARTESIAN_POINT('Ctrl Pts',(-43.123760117652,-5.19683028697976,-2.99647251163105));
#28089=CARTESIAN_POINT('Ctrl Pts',(-43.1701796656797,-5.54222062255303,
-2.07311227514093));
#28090=CARTESIAN_POINT('Ctrl Pts',(-43.2034113797181,-5.7894852632298,-1.41207948534963));
#28091=CARTESIAN_POINT('Ctrl Pts',(-43.2366430937566,-5.91591547937049,
-0.705847605549909));
#28092=CARTESIAN_POINT('Ctrl Pts',(-43.2698748077951,-5.91658768614795,
0.000149985469924119));
#28093=CARTESIAN_POINT('Ctrl Pts',(-43.5216251922048,-5.9164475069627,0.000129275767947919));
#28094=CARTESIAN_POINT('Ctrl Pts',(-43.4908325569335,-5.91592929355626,
-0.65409528884822));
#28095=CARTESIAN_POINT('Ctrl Pts',(-43.4600399216622,-5.80771341252565,
-1.30848705144103));
#28096=CARTESIAN_POINT('Ctrl Pts',(-43.4292472863909,-5.59476610119005,
-1.92680982644798));
#28097=CARTESIAN_POINT('Ctrl Pts',(-43.3828277383633,-5.27375044732369,
-2.85892438884555));
#28098=CARTESIAN_POINT('Ctrl Pts',(-43.3364081903356,-4.71473031238112,
-3.70907138287973));
#28099=CARTESIAN_POINT('Ctrl Pts',(-43.289988642308,-3.98613765091202,-4.37318081747182));
#28100=CARTESIAN_POINT('Ctrl Pts',(-43.2435690942804,-3.25754498944294,
-5.03729025206388));
#28101=CARTESIAN_POINT('Ctrl Pts',(-43.1971495462528,-2.35937980144735,
-5.51536212721385));
#28102=CARTESIAN_POINT('Ctrl Pts',(-43.1507299982252,-1.40159018267562,
-5.74887369787763));
#28103=CARTESIAN_POINT('Ctrl Pts',(-43.1043104501976,-0.443800563903852,
-5.98238526854141));
#28104=CARTESIAN_POINT('Ctrl Pts',(-43.05789090217,0.573613485644089,-5.97133653471901));
#28105=CARTESIAN_POINT('Ctrl Pts',(-43.0114713541424,1.52610612648058,-5.71708001737253));
#28106=CARTESIAN_POINT('Ctrl Pts',(-42.9650518061148,2.47859876731708,-5.46282350002606));
#28107=CARTESIAN_POINT('Ctrl Pts',(-42.9186322580871,3.36616999944212,-4.96535919915553));
#28108=CARTESIAN_POINT('Ctrl Pts',(-42.8722127100595,4.08016857682748,-4.2855837664187));
#28109=CARTESIAN_POINT('Ctrl Pts',(-42.8257931620319,4.79416715421282,-3.60580833368187));
#28110=CARTESIAN_POINT('Ctrl Pts',(-42.7793736140043,5.33459307685845,-2.74372176907874));
#28111=CARTESIAN_POINT('Ctrl Pts',(-42.7329540659767,5.63529058423927,-1.80485563564129));
#28112=CARTESIAN_POINT('Ctrl Pts',(-42.6865345179491,5.93598809162008,-0.865989502203833));
#28113=CARTESIAN_POINT('Ctrl Pts',(-42.6401149699215,5.99695718373608,0.149656200067966));
#28114=CARTESIAN_POINT('Ctrl Pts',(-42.5936954218938,5.81073438319206,1.1177521023516));
#28115=CARTESIAN_POINT('Ctrl Pts',(-42.5472758738662,5.62451158264803,2.08584800463521));
#28116=CARTESIAN_POINT('Ctrl Pts',(-42.5008563258386,5.19109688944399,3.00639410693068));
#28117=CARTESIAN_POINT('Ctrl Pts',(-42.454436777811,4.56354637926056,3.76670257369223));
#28118=CARTESIAN_POINT('Ctrl Pts',(-42.4080172297834,3.9359958690771,4.52701104045381));
#28119=CARTESIAN_POINT('Ctrl Pts',(-42.3615976817558,3.11430954191427,5.12708187168144));
#28120=CARTESIAN_POINT('Ctrl Pts',(-42.3151781337282,2.19907340153071,5.49345792820897));
#28121=CARTESIAN_POINT('Ctrl Pts',(-42.2687585857006,1.28383726114717,5.8598339847365));
#28122=CARTESIAN_POINT('Ctrl Pts',(-42.2223390376729,0.275051307542909,
5.99251526656391));
#28123=CARTESIAN_POINT('Ctrl Pts',(-42.1759194896453,-0.703794820515237,
5.87525971212658));
#28124=CARTESIAN_POINT('Ctrl Pts',(-42.1294999416177,-1.68264094857338,
5.75800415768925));
#28125=CARTESIAN_POINT('Ctrl Pts',(-42.0830803935901,-2.63154725108544,
5.39081176698717));
#28126=CARTESIAN_POINT('Ctrl Pts',(-42.0366608455625,-3.43435420372208,
4.81863207121049));
#28127=CARTESIAN_POINT('Ctrl Pts',(-41.9902412975349,-4.23716115635874,
4.2464523754338));
#28128=CARTESIAN_POINT('Ctrl Pts',(-41.9438217495072,-4.89386875911997,
3.46928537458253));
#28129=CARTESIAN_POINT('Ctrl Pts',(-41.8974022014796,-5.32408673263024,
2.58226727852723));
#28130=CARTESIAN_POINT('Ctrl Pts',(-41.8554765317214,-5.71265528721273,
1.78112143922053));
#28131=CARTESIAN_POINT('Ctrl Pts',(-41.8135508619631,-5.91646444995278,
0.890364337754753));
#28132=CARTESIAN_POINT('Ctrl Pts',(-41.7716251922048,-5.91713952097907,
-9.42380742528296E-5));
#28133=CARTESIAN_POINT('Origin',(-29.75,0.,0.));
#28134=CARTESIAN_POINT('',(-39.7698748077951,-5.91629469088874,7.39219476919573E-5));
#28135=CARTESIAN_POINT('',(-40.0216251922048,-5.91624628365206,2.79657000012922E-5));
#28136=CARTESIAN_POINT('',(-29.75,-5.91675,-7.2459289488551E-16));
#28137=CARTESIAN_POINT('Ctrl Pts',(-39.7698748077951,-5.91629469088874,
7.39219476919573E-5));
#28138=CARTESIAN_POINT('Ctrl Pts',(-39.7892406077606,-5.91647483503357,
0.411552807703675));
#28139=CARTESIAN_POINT('Ctrl Pts',(-39.808606407726,-5.87416701816864,0.822995174920484));
#28140=CARTESIAN_POINT('Ctrl Pts',(-39.8279722076915,-5.78899689027189,
1.22536481866197));
#28141=CARTESIAN_POINT('Ctrl Pts',(-39.8743917557191,-5.58484530089954,
2.18983915154763));
#28142=CARTESIAN_POINT('Ctrl Pts',(-39.9208113037468,-5.13442654398146,
3.10218577926745));
#28143=CARTESIAN_POINT('Ctrl Pts',(-39.9672308517744,-4.4928782325929,3.85072059769141));
#28144=CARTESIAN_POINT('Ctrl Pts',(-40.013650399802,-3.85132992120435,4.59925541611538));
#28145=CARTESIAN_POINT('Ctrl Pts',(-40.0600699478296,-3.01865205534533,
5.18397842524349));
#28146=CARTESIAN_POINT('Ctrl Pts',(-40.1064894958572,-2.09677615824598,
5.53331127595433));
#28147=CARTESIAN_POINT('Ctrl Pts',(-40.1529090438848,-1.17490026114667,
5.88264412666515));
#28148=CARTESIAN_POINT('Ctrl Pts',(-40.1993285919124,-0.163826332807044,
5.99658681895872));
#28149=CARTESIAN_POINT('Ctrl Pts',(-40.2457481399401,0.812675907605946,
5.86119115910656));
#28150=CARTESIAN_POINT('Ctrl Pts',(-40.2921676879677,1.78917814801902,5.72579549925439));
#28151=CARTESIAN_POINT('Ctrl Pts',(-40.3385872359953,2.73110870050545,5.34106148725645));
#28152=CARTESIAN_POINT('Ctrl Pts',(-40.3850067840229,3.52316197099507,4.75408599633264));
#28153=CARTESIAN_POINT('Ctrl Pts',(-40.4314263320505,4.31521524148466,4.16711050540887));
#28154=CARTESIAN_POINT('Ctrl Pts',(-40.4778458800781,4.95739122997746,3.37789353555927));
#28155=CARTESIAN_POINT('Ctrl Pts',(-40.5242654281057,5.37107853178416,2.48304638293356));
#28156=CARTESIAN_POINT('Ctrl Pts',(-40.5706849761334,5.78476583359088,1.5881992303078));
#28157=CARTESIAN_POINT('Ctrl Pts',(-40.617104524161,5.96996444871147,0.58772189490592));
#28158=CARTESIAN_POINT('Ctrl Pts',(-40.6635240721886,5.90400345275445,-0.395913076641409));
#28159=CARTESIAN_POINT('Ctrl Pts',(-40.7099436202162,5.83804245679743,-1.37954804818868));
#28160=CARTESIAN_POINT('Ctrl Pts',(-40.7563631682438,5.52092184976282,-2.34634065588141));
#28161=CARTESIAN_POINT('Ctrl Pts',(-40.8027827162714,4.99146166980471,-3.17794183918814));
#28162=CARTESIAN_POINT('Ctrl Pts',(-40.849202264299,4.46200148984657,-4.0095430224949));
#28163=CARTESIAN_POINT('Ctrl Pts',(-40.8956218123267,3.72020173696491,-4.70595278141567));
#28164=CARTESIAN_POINT('Ctrl Pts',(-40.9420413603543,2.85686917070408,-5.1819207323031));
#28165=CARTESIAN_POINT('Ctrl Pts',(-40.9884609083819,1.99353660444324,-5.65788868319053));
#28166=CARTESIAN_POINT('Ctrl Pts',(-41.0348804564094,1.00867122480323,-5.91341482604464));
#28167=CARTESIAN_POINT('Ctrl Pts',(-41.0813000044371,0.022834454681672,
-5.91721915447378));
#28168=CARTESIAN_POINT('Ctrl Pts',(-41.1277195524647,-0.963002315439857,
-5.92102348290293));
#28169=CARTESIAN_POINT('Ctrl Pts',(-41.1741391004923,-1.94981047604293,
-5.67310599690714));
#28170=CARTESIAN_POINT('Ctrl Pts',(-41.2205586485199,-2.81679078041956,
-5.20381529588968));
#28171=CARTESIAN_POINT('Ctrl Pts',(-41.2669781965476,-3.68377108479622,
-4.73452459487222));
#28172=CARTESIAN_POINT('Ctrl Pts',(-41.3133977445751,-4.43092353294642,
-4.04386067883307));
#28173=CARTESIAN_POINT('Ctrl Pts',(-41.3598172926028,-4.96678611987679,
-3.21637055915381));
#28174=CARTESIAN_POINT('Ctrl Pts',(-41.4062368406304,-5.50264870680715,
-2.38888043947455));
#28175=CARTESIAN_POINT('Ctrl Pts',(-41.452656388658,-5.82722143251769,-1.42456411615518));
#28176=CARTESIAN_POINT('Ctrl Pts',(-41.4990759366856,-5.90077201434889,
-0.441467517569472));
#28177=CARTESIAN_POINT('Ctrl Pts',(-41.5060088937221,-5.91175710674018,
-0.294637856999195));
#28178=CARTESIAN_POINT('Ctrl Pts',(-41.5129418507586,-5.9171427250718,-0.147389270582132));
#28179=CARTESIAN_POINT('Ctrl Pts',(-41.5198748077951,-5.91700124842561,
-0.000130358588716351));
#28180=CARTESIAN_POINT('Ctrl Pts',(-41.7716251922048,-5.91713952097907,
-9.42380742528296E-5));
#28181=CARTESIAN_POINT('Ctrl Pts',(-41.7671313139355,-5.91721187968038,
-0.0955396410157708));
#28182=CARTESIAN_POINT('Ctrl Pts',(-41.7626374356662,-5.91495042886566,
-0.1909816141934));
#28183=CARTESIAN_POINT('Ctrl Pts',(-41.7581435573968,-5.91033254064073,
-0.286309436388467));
#28184=CARTESIAN_POINT('Ctrl Pts',(-41.7117240093692,-5.86263203088166,
-1.27099886398967));
#28185=CARTESIAN_POINT('Ctrl Pts',(-41.6653044613416,-5.56350266710422,
-2.24350852793274));
#28186=CARTESIAN_POINT('Ctrl Pts',(-41.618884913314,-5.04956210535865,-3.08478951931048));
#28187=CARTESIAN_POINT('Ctrl Pts',(-41.5724653652863,-4.5356215436131,-3.92607051068819));
#28188=CARTESIAN_POINT('Ctrl Pts',(-41.5260458172587,-3.80686978389939,
-4.63612282950058));
#28189=CARTESIAN_POINT('Ctrl Pts',(-41.4796262692311,-2.9525163272383,-5.12802605021787));
#28190=CARTESIAN_POINT('Ctrl Pts',(-41.4332067212035,-2.09816287057719,
-5.61992927093518));
#28191=CARTESIAN_POINT('Ctrl Pts',(-41.3867871731759,-1.11820771696867,
-5.89368339355742));
#28192=CARTESIAN_POINT('Ctrl Pts',(-41.3403676251483,-0.132611208340943,
-5.9157770496989));
#28193=CARTESIAN_POINT('Ctrl Pts',(-41.2939480771207,0.852985300286781,
-5.93787070584039));
#28194=CARTESIAN_POINT('Ctrl Pts',(-41.2475285290931,1.84422316393366,-5.70830389550112));
#28195=CARTESIAN_POINT('Ctrl Pts',(-41.2011089810655,2.71976087771816,-5.25517883638184));
#28196=CARTESIAN_POINT('Ctrl Pts',(-41.1546894330379,3.59529859150262,-4.80205377726258));
#28197=CARTESIAN_POINT('Ctrl Pts',(-41.1082698850102,4.35513615542474,-4.1253704693633));
#28198=CARTESIAN_POINT('Ctrl Pts',(-41.0618503369826,4.90625872728235,-3.30796450030643));
#28199=CARTESIAN_POINT('Ctrl Pts',(-41.015430788955,5.45738129914,-2.49055853124952));
#28200=CARTESIAN_POINT('Ctrl Pts',(-40.9690112409274,5.79978887893315,-1.53242990103499));
#28201=CARTESIAN_POINT('Ctrl Pts',(-40.9225916928998,5.89156594614075,-0.5508670770672));
#28202=CARTESIAN_POINT('Ctrl Pts',(-40.8761721448722,5.98334301334835,0.430695746900592));
#28203=CARTESIAN_POINT('Ctrl Pts',(-40.8297525968445,5.82448956797039,1.4356927646216));
#28204=CARTESIAN_POINT('Ctrl Pts',(-40.7833330488169,5.43445151378507,2.34109815655837));
#28205=CARTESIAN_POINT('Ctrl Pts',(-40.7369135007893,5.04441345959976,3.24650354849512));
#28206=CARTESIAN_POINT('Ctrl Pts',(-40.6904939527617,4.42319079660706,4.05231731464766));
#28207=CARTESIAN_POINT('Ctrl Pts',(-40.6440744047341,3.64682994671907,4.65989647675084));
#28208=CARTESIAN_POINT('Ctrl Pts',(-40.5976548567065,2.87046909683105,5.26747563885403));
#28209=CARTESIAN_POINT('Ctrl Pts',(-40.5512353086789,1.93897006004773,5.67682019690788));
#28210=CARTESIAN_POINT('Ctrl Pts',(-40.5048157606513,0.966361465686305,
5.83782059950102));
#28211=CARTESIAN_POINT('Ctrl Pts',(-40.4583962126236,-0.00624712867508953,
5.99882100209416));
#28212=CARTESIAN_POINT('Ctrl Pts',(-40.411976664596,-1.01996528061453,5.91147724922659));
#28213=CARTESIAN_POINT('Ctrl Pts',(-40.3655571165684,-1.95069958067579,
5.58648144902255));
#28214=CARTESIAN_POINT('Ctrl Pts',(-40.3191375685408,-2.88143388073706,
5.26148564881852));
#28215=CARTESIAN_POINT('Ctrl Pts',(-40.2727180205132,-3.72918432892018,
4.69883780127797));
#28216=CARTESIAN_POINT('Ctrl Pts',(-40.2262984724856,-4.39017430518342,
3.96741394417436));
#28217=CARTESIAN_POINT('Ctrl Pts',(-40.179878924458,-5.05116428144667,3.23599008707073));
#28218=CARTESIAN_POINT('Ctrl Pts',(-40.1334593764304,-5.52539378579008,
2.33579022040401));
#28219=CARTESIAN_POINT('Ctrl Pts',(-40.0870398284027,-5.75481043358768,
1.37701151331141));
#28220=CARTESIAN_POINT('Ctrl Pts',(-40.0652349496701,-5.86257542478278,
0.926639755551992));
#28221=CARTESIAN_POINT('Ctrl Pts',(-40.0434300709375,-5.91632225961091,
0.463342528899467));
#28222=CARTESIAN_POINT('Ctrl Pts',(-40.0216251922048,-5.91624628365206,
2.79657000012922E-5));
#28223=CARTESIAN_POINT('Origin',(-29.75,0.,0.));
#28224=CARTESIAN_POINT('',(-38.0198748077951,-5.91725909577585,-1.71678216764892E-5));
#28225=CARTESIAN_POINT('',(-38.2716251922048,-5.91724351279131,3.79183957586531E-5));
#28226=CARTESIAN_POINT('',(-29.75,-5.91675,-7.2459289488551E-16));
#28227=CARTESIAN_POINT('Ctrl Pts',(-38.0198748077951,-5.91725909577585,
-1.71678216764892E-5));
#28228=CARTESIAN_POINT('Ctrl Pts',(-38.0655393647625,-5.91709852423039,
0.969794642514453));
#28229=CARTESIAN_POINT('Ctrl Pts',(-38.11120392173,-5.67381360263478,1.93968406368008));
#28230=CARTESIAN_POINT('Ctrl Pts',(-38.1568684786975,-5.21580439043804,
2.79452831352257));
#28231=CARTESIAN_POINT('Ctrl Pts',(-38.2032880267251,-4.75022272197246,
3.66350605790234));
#28232=CARTESIAN_POINT('Ctrl Pts',(-38.2497075747527,-4.06275781569343,
4.41360300385667));
#28233=CARTESIAN_POINT('Ctrl Pts',(-38.2961271227803,-3.2375650790368,4.9529966983023));
#28234=CARTESIAN_POINT('Ctrl Pts',(-38.342546670808,-2.41237234238023,5.49239039274791));
#28235=CARTESIAN_POINT('Ctrl Pts',(-38.3889662188356,-1.44945177534604,
5.82108083568479));
#28236=CARTESIAN_POINT('Ctrl Pts',(-38.4353857668632,-0.466678446039116,
5.89883167774726));
#28237=CARTESIAN_POINT('Ctrl Pts',(-38.4818053148908,0.516094883267838,
5.97658251980974));
#28238=CARTESIAN_POINT('Ctrl Pts',(-38.5282248629184,1.51872097484763,5.80339376099782));
#28239=CARTESIAN_POINT('Ctrl Pts',(-38.574644410946,2.41846424398577,5.40046614978322));
#28240=CARTESIAN_POINT('Ctrl Pts',(-38.6210639589736,3.31820751312388,4.99753853856864));
#28241=CARTESIAN_POINT('Ctrl Pts',(-38.6674835070012,4.11506795982038,4.36487207495137));
#28242=CARTESIAN_POINT('Ctrl Pts',(-38.7139030550289,4.7114986184791,3.57991406355817));
#28243=CARTESIAN_POINT('Ctrl Pts',(-38.7603226030565,5.30792927713784,2.79495605216495));
#28244=CARTESIAN_POINT('Ctrl Pts',(-38.8067421510841,5.70393014775882,1.85770649299578));
#28245=CARTESIAN_POINT('Ctrl Pts',(-38.8531616991117,5.85102513460574,0.882897960471064));
#28246=CARTESIAN_POINT('Ctrl Pts',(-38.8995812471393,5.99812012145267,-0.0919105720536834));
#28247=CARTESIAN_POINT('Ctrl Pts',(-38.9460007951669,5.89630922452556,-1.10427807793392));
#28248=CARTESIAN_POINT('Ctrl Pts',(-38.9924203431945,5.55805553457138,-2.03027648585422));
#28249=CARTESIAN_POINT('Ctrl Pts',(-39.0388398912221,5.21980184461722,-2.95627489377446));
#28250=CARTESIAN_POINT('Ctrl Pts',(-39.0852594392497,4.64510536163601,-3.79590420373472));
#28251=CARTESIAN_POINT('Ctrl Pts',(-39.1316789872773,3.904317046434,-4.4463819376339));
#28252=CARTESIAN_POINT('Ctrl Pts',(-39.178098535305,3.16352873123197,-5.09685967153309));
#28253=CARTESIAN_POINT('Ctrl Pts',(-39.2245180833326,2.25664858380911,-5.5581858293712));
#28254=CARTESIAN_POINT('Ctrl Pts',(-39.2709376313602,1.29469153395299,-5.77388757825284));
#28255=CARTESIAN_POINT('Ctrl Pts',(-39.3173571793878,0.332734484096863,
-5.98958932713449));
#28256=CARTESIAN_POINT('Ctrl Pts',(-39.3637767274154,-0.684299468192547,
-5.95966666705966));
#28257=CARTESIAN_POINT('Ctrl Pts',(-39.4101962754431,-1.63191101269678,
-5.68778255395115));
#28258=CARTESIAN_POINT('Ctrl Pts',(-39.4566158234707,-2.57952255720101,
-5.41589844084264));
#28259=CARTESIAN_POINT('Ctrl Pts',(-39.5030353714982,-3.45771169392008,
-4.90205287470045));
#28260=CARTESIAN_POINT('Ctrl Pts',(-39.5494549195259,-4.15897567772266,
-4.20914780525743));
#28261=CARTESIAN_POINT('Ctrl Pts',(-39.5958744675535,-4.86023966152524,
-3.51624273581441));
#28262=CARTESIAN_POINT('Ctrl Pts',(-39.6422940155811,-5.38457849241134,
-2.64427816307056));
#28263=CARTESIAN_POINT('Ctrl Pts',(-39.6887135636087,-5.66780569694108,
-1.69999485767289));
#28264=CARTESIAN_POINT('Ctrl Pts',(-39.7157673116709,-5.83287316875554,
-1.14965768876502));
#28265=CARTESIAN_POINT('Ctrl Pts',(-39.742821059733,-5.91604303207176,-0.574756249176902));
#28266=CARTESIAN_POINT('Ctrl Pts',(-39.7698748077951,-5.91629469088874,
7.39219476919573E-5));
#28267=CARTESIAN_POINT('Ctrl Pts',(-40.0216251922048,-5.91624628365206,
2.79657000012922E-5));
#28268=CARTESIAN_POINT('Ctrl Pts',(-39.9970105229098,-5.91616051738276,
-0.522989607226258));
#28269=CARTESIAN_POINT('Ctrl Pts',(-39.9723958536149,-5.84748692575974,
-1.04602927257089));
#28270=CARTESIAN_POINT('Ctrl Pts',(-39.9477811843199,-5.71050652059654,
-1.55052220640218));
#28271=CARTESIAN_POINT('Ctrl Pts',(-39.9013616362923,-5.452182168556,-2.50191967150481));
#28272=CARTESIAN_POINT('Ctrl Pts',(-39.8549420882647,-4.95092967322311,
-3.38735705419161));
#28273=CARTESIAN_POINT('Ctrl Pts',(-39.8085225402371,-4.26810941472458,
-4.09844432172273));
#28274=CARTESIAN_POINT('Ctrl Pts',(-39.7621029922095,-3.58528915622607,
-4.80953158925383));
#28275=CARTESIAN_POINT('Ctrl Pts',(-39.7156834441818,-2.72090113456196,
-5.34626874162926));
#28276=CARTESIAN_POINT('Ctrl Pts',(-39.6692638961542,-1.78075864359127,
-5.6429515758685));
#28277=CARTESIAN_POINT('Ctrl Pts',(-39.6228443481266,-0.840616152620568,
-5.93963441010775));
#28278=CARTESIAN_POINT('Ctrl Pts',(-39.576424800099,0.175280807656705,-5.99626292621078));
#28279=CARTESIAN_POINT('Ctrl Pts',(-39.5300052520714,1.14257211089189,-5.80590499454942));
#28280=CARTESIAN_POINT('Ctrl Pts',(-39.4835857040438,2.10986341412708,-5.61554706288806));
#28281=CARTESIAN_POINT('Ctrl Pts',(-39.4371661560162,3.02854906032023,-5.17820268346229));
#28282=CARTESIAN_POINT('Ctrl Pts',(-39.3907466079886,3.786168960011,-4.54740898101007));
#28283=CARTESIAN_POINT('Ctrl Pts',(-39.3443270599609,4.54378885970176,-3.91661527855786));
#28284=CARTESIAN_POINT('Ctrl Pts',(-39.2979075119333,5.14034301289013,-3.09237225307922));
#28285=CARTESIAN_POINT('Ctrl Pts',(-39.2514879639057,5.50280477143654,-2.17557888429198));
#28286=CARTESIAN_POINT('Ctrl Pts',(-39.2050684158781,5.86526652998294,-1.25878551550473));
#28287=CARTESIAN_POINT('Ctrl Pts',(-39.1586488678505,5.99363589388735,-0.249441803408889));
#28288=CARTESIAN_POINT('Ctrl Pts',(-39.1122293198229,5.87219864119747,0.728894335717105));
#28289=CARTESIAN_POINT('Ctrl Pts',(-39.0658097717953,5.75076138850759,1.7072304748431));
#28290=CARTESIAN_POINT('Ctrl Pts',(-39.0193902237677,5.37951751922341,2.65455904099929));
#28291=CARTESIAN_POINT('Ctrl Pts',(-38.97297067574,4.80391252269629,3.45491364705453));
#28292=CARTESIAN_POINT('Ctrl Pts',(-38.9265511277124,4.22830752616917,4.25526825310977));
#28293=CARTESIAN_POINT('Ctrl Pts',(-38.8801315796848,3.44834140239914,4.90864889906404));
#28294=CARTESIAN_POINT('Ctrl Pts',(-38.8337120316572,2.5594930134089,5.33507257201182));
#28295=CARTESIAN_POINT('Ctrl Pts',(-38.7872924836296,1.67064462441864,5.76149624495962));
#28296=CARTESIAN_POINT('Ctrl Pts',(-38.740872935602,0.672913970208175,5.96096294490088));
#28297=CARTESIAN_POINT('Ctrl Pts',(-38.6944533875744,-0.311562635136377,
5.90905513248174));
#28298=CARTESIAN_POINT('Ctrl Pts',(-38.6480338395467,-1.2960392404809,5.85714732006259));
#28299=CARTESIAN_POINT('Ctrl Pts',(-38.6016142915191,-2.26726179695949,
5.55386499528307));
#28300=CARTESIAN_POINT('Ctrl Pts',(-38.5551947434915,-3.10633895578493,
5.03633419523514));
#28301=CARTESIAN_POINT('Ctrl Pts',(-38.5087751954639,-3.94541611461034,
4.51880339518723));
#28302=CARTESIAN_POINT('Ctrl Pts',(-38.4623556474363,-4.65234787578258,
3.7870241198709));
#28303=CARTESIAN_POINT('Ctrl Pts',(-38.4159360994087,-5.14059581407073,
2.93057648094711));
#28304=CARTESIAN_POINT('Ctrl Pts',(-38.3695165513811,-5.6288437523589,2.0741288420233));
#28305=CARTESIAN_POINT('Ctrl Pts',(-38.3230970033535,-5.89840786776299,
1.09301283949197));
#28306=CARTESIAN_POINT('Ctrl Pts',(-38.2766774553259,-5.91628970791874,
0.107330919573857));
#28307=CARTESIAN_POINT('Ctrl Pts',(-38.2749933676188,-5.91693845588085,
0.0715706660839549));
#28308=CARTESIAN_POINT('Ctrl Pts',(-38.2733092799118,-5.91725593527694,
0.0358044028545749));
#28309=CARTESIAN_POINT('Ctrl Pts',(-38.2716251922048,-5.91724351279131,
3.7918395758653E-5));
#28310=CARTESIAN_POINT('Origin',(-29.75,0.,0.));
#28311=CARTESIAN_POINT('',(-36.2698748077951,-5.91625954349593,-4.60302636559606E-5));
#28312=CARTESIAN_POINT('',(-36.5216251922048,-5.91632433790914,-8.97973128488559E-5));
#28313=CARTESIAN_POINT('',(-29.75,-5.91675,-7.2459289488551E-16));
#28314=CARTESIAN_POINT('Ctrl Pts',(-36.2698748077951,-5.91625954349593,
-4.60302636559606E-5));
#28315=CARTESIAN_POINT('Ctrl Pts',(-36.2954185737369,-5.91611265376947,
0.542709703882021));
#28316=CARTESIAN_POINT('Ctrl Pts',(-36.3209623396788,-5.84208692011566,
1.0855047064104));
#28317=CARTESIAN_POINT('Ctrl Pts',(-36.3465061056206,-5.69470404581093,
1.60759129290275));
#28318=CARTESIAN_POINT('Ctrl Pts',(-36.3929256536482,-5.4268717133423,2.55635599077197));
#28319=CARTESIAN_POINT('Ctrl Pts',(-36.4393452016758,-4.91678348370265,
3.43673285534667));
#28320=CARTESIAN_POINT('Ctrl Pts',(-36.4857647497034,-4.22688135560573,
4.14095133272836));
#28321=CARTESIAN_POINT('Ctrl Pts',(-36.5321842977311,-3.53697922750878,
4.84516981011006));
#28322=CARTESIAN_POINT('Ctrl Pts',(-36.5786038457587,-2.66726320095454,
5.37322990029873));
#28323=CARTESIAN_POINT('Ctrl Pts',(-36.6250233937863,-1.72419879280033,
5.66048959519386));
#28324=CARTESIAN_POINT('Ctrl Pts',(-36.6714429418139,-0.781134384646113,
5.94774929008899));
#28325=CARTESIAN_POINT('Ctrl Pts',(-36.7178624898415,0.235278405108075,
5.99420858969058));
#28326=CARTESIAN_POINT('Ctrl Pts',(-36.7642820378691,1.20061630530521,5.79418021999897));
#28327=CARTESIAN_POINT('Ctrl Pts',(-36.8107015858967,2.16595420550232,5.59415185030736));
#28328=CARTESIAN_POINT('Ctrl Pts',(-36.8571211339243,3.08021721614238,5.14763581132257));
#28329=CARTESIAN_POINT('Ctrl Pts',(-36.903540681952,3.83148664077805,4.50929196836171));
#28330=CARTESIAN_POINT('Ctrl Pts',(-36.9499602299796,4.58275606541374,3.87094812540083));
#28331=CARTESIAN_POINT('Ctrl Pts',(-36.9963797780072,5.17103190404502,3.04077647846387));
#28332=CARTESIAN_POINT('Ctrl Pts',(-37.0427993260348,5.52430089107451,2.12040175421203));
#28333=CARTESIAN_POINT('Ctrl Pts',(-37.0892188740624,5.877569878104,1.20002702996018));
#28334=CARTESIAN_POINT('Ctrl Pts',(-37.13563842209,5.99583201353171,0.189449228393454));
#28335=CARTESIAN_POINT('Ctrl Pts',(-37.1820579701176,5.86461034282473,-0.787622664240537));
#28336=CARTESIAN_POINT('Ctrl Pts',(-37.2284775181453,5.73338867211774,-1.76469455687453));
#28337=CARTESIAN_POINT('Ctrl Pts',(-37.2748970661728,5.35268319527606,-2.70826054057578));
#28338=CARTESIAN_POINT('Ctrl Pts',(-37.3213166142005,4.76909763595757,-3.50281482141091));
#28339=CARTESIAN_POINT('Ctrl Pts',(-37.3677361622281,4.18551207663908,-4.29736910224604));
#28340=CARTESIAN_POINT('Ctrl Pts',(-37.4141557102557,3.39904643484378,-4.94291168021504));
#28341=CARTESIAN_POINT('Ctrl Pts',(-37.4605752582833,2.50597520533521,-5.36041903256053));
#28342=CARTESIAN_POINT('Ctrl Pts',(-37.5069948063109,1.61290397582666,-5.77792638490601));
#28343=CARTESIAN_POINT('Ctrl Pts',(-37.5534143543385,0.613227158604841,
-5.96739851162799));
#28344=CARTESIAN_POINT('Ctrl Pts',(-37.5998339023661,-0.370680694423386,
-5.90564135019846));
#28345=CARTESIAN_POINT('Ctrl Pts',(-37.6462534503937,-1.35458854745164,
-5.84388418876892));
#28346=CARTESIAN_POINT('Ctrl Pts',(-37.6926729984214,-2.3227274362863,-5.53089773918786));
#28347=CARTESIAN_POINT('Ctrl Pts',(-37.739092546449,-3.15658349658267,-5.00499596038738));
#28348=CARTESIAN_POINT('Ctrl Pts',(-37.7855120944766,-3.99043955687904,
-4.47909418158689));
#28349=CARTESIAN_POINT('Ctrl Pts',(-37.8319316425042,-4.69001278863712,
-3.74027707356698));
#28350=CARTESIAN_POINT('Ctrl Pts',(-37.8783511905318,-5.16966555448492,
-2.87898627804374));
#28351=CARTESIAN_POINT('Ctrl Pts',(-37.9247707385594,-5.64931832033271,
-2.01769548252052));
#28352=CARTESIAN_POINT('Ctrl Pts',(-37.971190286587,-5.90905062027022,-1.03393099949398));
#28353=CARTESIAN_POINT('Ctrl Pts',(-38.0176098346146,-5.91706755491295,
-0.0481194865781631));
#28354=CARTESIAN_POINT('Ctrl Pts',(-38.0183648256748,-5.91719794640193,
-0.032085748403995));
#28355=CARTESIAN_POINT('Ctrl Pts',(-38.0191198167349,-5.91726175057181,
-0.0160514687204437));
#28356=CARTESIAN_POINT('Ctrl Pts',(-38.0198748077951,-5.91725909577585,
-1.71678216764892E-5));
#28357=CARTESIAN_POINT('Ctrl Pts',(-38.2716251922048,-5.91724351279131,
3.7918395758653E-5));
#28358=CARTESIAN_POINT('Ctrl Pts',(-38.2268897318842,-5.91691352664454,
-0.95004926510235));
#28359=CARTESIAN_POINT('Ctrl Pts',(-38.1821542715636,-5.68379628383804,
-1.90029255378405));
#28360=CARTESIAN_POINT('Ctrl Pts',(-38.137418811243,-5.24350887576506,-2.74219228065701));
#28361=CARTESIAN_POINT('Ctrl Pts',(-38.0909992632154,-4.78664663854823,
-3.61578572366473));
#28362=CARTESIAN_POINT('Ctrl Pts',(-38.0445797151878,-4.10672259920717,
-4.37272477237521));
#28363=CARTESIAN_POINT('Ctrl Pts',(-37.9981601671602,-3.28696905663254,
-4.92034940375804));
#28364=CARTESIAN_POINT('Ctrl Pts',(-37.9517406191326,-2.46721551405795,
-5.46797403514083));
#28365=CARTESIAN_POINT('Ctrl Pts',(-37.9053210711049,-1.50763246824981,
-5.806284249196));
#28366=CARTESIAN_POINT('Ctrl Pts',(-37.8589015230773,-0.525686427608837,
-5.89386610079917));
#28367=CARTESIAN_POINT('Ctrl Pts',(-37.8124819750497,0.456259613032197,
-5.98144795240236));
#28368=CARTESIAN_POINT('Ctrl Pts',(-37.7660624270221,1.46056864850614,-5.81830144155351));
#28369=CARTESIAN_POINT('Ctrl Pts',(-37.7196428789945,2.36429907801261,-5.42439800383698));
#28370=CARTESIAN_POINT('Ctrl Pts',(-37.6732233309669,3.26802950751907,-5.03049456612045));
#28371=CARTESIAN_POINT('Ctrl Pts',(-37.6268037829393,4.07118133105807,-4.40583420153629));
#28372=CARTESIAN_POINT('Ctrl Pts',(-37.5803842349117,4.67543742971133,-3.62688415519109));
#28373=CARTESIAN_POINT('Ctrl Pts',(-37.533964686884,5.27969352836458,-2.84793410884589));
#28374=CARTESIAN_POINT('Ctrl Pts',(-37.4875451388564,5.68505390213202,-1.91469438073971));
#28375=CARTESIAN_POINT('Ctrl Pts',(-37.4411255908288,5.84189671999184,-0.941406685375875));
#28376=CARTESIAN_POINT('Ctrl Pts',(-37.3947060428012,5.99873953785166,0.0318810099879278));
#28377=CARTESIAN_POINT('Ctrl Pts',(-37.3482864947736,5.90706479980387,1.04521667260943));
#28378=CARTESIAN_POINT('Ctrl Pts',(-37.301866946746,5.57809478768647,1.97455371512322));
#28379=CARTESIAN_POINT('Ctrl Pts',(-37.2554473987184,5.24912477556906,2.90389075763703));
#28380=CARTESIAN_POINT('Ctrl Pts',(-37.2090278506908,4.68285948938204,3.74922918004318));
#28381=CARTESIAN_POINT('Ctrl Pts',(-37.1626083026632,3.94861779244578,4.40708762829858));
#28382=CARTESIAN_POINT('Ctrl Pts',(-37.1161887546355,3.21437609550952,5.06494607655399));
#28383=CARTESIAN_POINT('Ctrl Pts',(-37.0697692066079,2.31215798782404,5.53532455065863));
#28384=CARTESIAN_POINT('Ctrl Pts',(-37.0233496585803,1.35240769971278,5.76064208644136));
#28385=CARTESIAN_POINT('Ctrl Pts',(-36.9769301105527,0.39265741160152,5.98595962222409));
#28386=CARTESIAN_POINT('Ctrl Pts',(-36.9305105625251,-0.624625056935495,
5.96621621968489));
#28387=CARTESIAN_POINT('Ctrl Pts',(-36.8840910144975,-1.57490997378356,
5.70382874995375));
#28388=CARTESIAN_POINT('Ctrl Pts',(-36.8376714664699,-2.5251948906316,5.44144128022261));
#28389=CARTESIAN_POINT('Ctrl Pts',(-36.7912519184422,-3.40848225579067,
4.93640974329955));
#28390=CARTESIAN_POINT('Ctrl Pts',(-36.7448323704146,-4.11664522901183,
4.25055712733942));
#28391=CARTESIAN_POINT('Ctrl Pts',(-36.698412822387,-4.82480820223301,3.56470451137927));
#28392=CARTESIAN_POINT('Ctrl Pts',(-36.6519932743594,-5.35784678351626,
2.69803081638205));
#28393=CARTESIAN_POINT('Ctrl Pts',(-36.6055737263318,-5.65050952718447,
1.75662913488289));
#28394=CARTESIAN_POINT('Ctrl Pts',(-36.5775908816228,-5.82693382376107,
1.18912905826634));
#28395=CARTESIAN_POINT('Ctrl Pts',(-36.5496080369138,-5.91600614704412,
0.594473019777904));
#28396=CARTESIAN_POINT('Ctrl Pts',(-36.5216251922048,-5.91632433790914,
-8.97973128488559E-5));
#28397=CARTESIAN_POINT('Origin',(-29.75,0.,0.));
#28398=CARTESIAN_POINT('',(-34.5198748077951,-5.9170907741469,0.000109654298403733));
#28399=CARTESIAN_POINT('',(-34.7716251922048,-5.91694163414713,0.000140169273084226));
#28400=CARTESIAN_POINT('',(-29.75,-5.91675,-7.2459289488551E-16));
#28401=CARTESIAN_POINT('Ctrl Pts',(-34.5198748077951,-5.9170907741469,0.000109654298403733));
#28402=CARTESIAN_POINT('Ctrl Pts',(-34.5252977827113,-5.91718880965865,
0.11529087392914));
#28403=CARTESIAN_POINT('Ctrl Pts',(-34.5307207576275,-5.91389496019476,
0.230466490326725));
#28404=CARTESIAN_POINT('Ctrl Pts',(-34.5361437325437,-5.9071714106131,0.345441543574822));
#28405=CARTESIAN_POINT('Ctrl Pts',(-34.5825632805713,-5.849619211397,1.32960431192358));
#28406=CARTESIAN_POINT('Ctrl Pts',(-34.628982828599,-5.54077263440303,2.29907180368102));
#28407=CARTESIAN_POINT('Ctrl Pts',(-34.6754023766266,-5.0184388597283,3.13516751475276));
#28408=CARTESIAN_POINT('Ctrl Pts',(-34.7218219246542,-4.49610508505359,
3.97126322582447));
#28409=CARTESIAN_POINT('Ctrl Pts',(-34.7682414726818,-3.76028411269806,
4.67398715621054));
#28410=CARTESIAN_POINT('Ctrl Pts',(-34.8146610207094,-2.90105081508504,
5.1573159785577));
#28411=CARTESIAN_POINT('Ctrl Pts',(-34.861080568737,-2.04181751747196,5.64064480090488));
#28412=CARTESIAN_POINT('Ctrl Pts',(-34.9075001167646,-1.0591718946014,5.90457851521318));
#28413=CARTESIAN_POINT('Ctrl Pts',(-34.9539196647922,-0.0734036398125114,
5.91680790968021));
#28414=CARTESIAN_POINT('Ctrl Pts',(-35.0003392128198,0.912364614976294,
5.92903730414724));
#28415=CARTESIAN_POINT('Ctrl Pts',(-35.0467587608474,1.90125550168333,5.68956237877302));
#28416=CARTESIAN_POINT('Ctrl Pts',(-35.0931783088751,2.77221481852983,5.2276982443821));
#28417=CARTESIAN_POINT('Ctrl Pts',(-35.1395978569027,3.64317413537638,4.76583410999116));
#28418=CARTESIAN_POINT('Ctrl Pts',(-35.1860174049303,4.39620188236236,4.08158076658348));
#28419=CARTESIAN_POINT('Ctrl Pts',(-35.2324369529579,4.9391168349927,3.25870048097148));
#28420=CARTESIAN_POINT('Ctrl Pts',(-35.2788565009855,5.48203178762306,2.43582019535944));
#28421=CARTESIAN_POINT('Ctrl Pts',(-35.3252760490131,5.81483394589777,1.47431296754308));
#28422=CARTESIAN_POINT('Ctrl Pts',(-35.3716955970407,5.8967836284609,0.49188085295889));
#28423=CARTESIAN_POINT('Ctrl Pts',(-35.4181151450684,5.97873331102404,-0.490551261625275));
#28424=CARTESIAN_POINT('Ctrl Pts',(-35.464534693096,5.8098305178756,-1.49390826297733));
#28425=CARTESIAN_POINT('Ctrl Pts',(-35.5109542411236,5.41075133479782,-2.39536509271044));
#28426=CARTESIAN_POINT('Ctrl Pts',(-35.5573737891512,5.01167215172005,-3.29682192244353));
#28427=CARTESIAN_POINT('Ctrl Pts',(-35.6037933371788,4.38241657871295,-4.09637858055776));
#28428=CARTESIAN_POINT('Ctrl Pts',(-35.6502128852064,3.60001437925112,-4.69615804712504));
#28429=CARTESIAN_POINT('Ctrl Pts',(-35.696632433234,2.81761217978926,-5.29593751369234));
#28430=CARTESIAN_POINT('Ctrl Pts',(-35.7430519812617,1.88206335387267,-5.69593978871267));
#28431=CARTESIAN_POINT('Ctrl Pts',(-35.7894715292893,0.907892282167387,
-5.84719894807531));
#28432=CARTESIAN_POINT('Ctrl Pts',(-35.8358910773169,-0.0662787895378396,
-5.99845810743793));
#28433=CARTESIAN_POINT('Ctrl Pts',(-35.8823106253445,-1.07907210703174,
-5.90097415114289));
#28434=CARTESIAN_POINT('Ctrl Pts',(-35.9287301733721,-2.00650747364734,
-5.56668049133318));
#28435=CARTESIAN_POINT('Ctrl Pts',(-35.9751497213997,-2.93394284026303,
-5.23238683152344));
#28436=CARTESIAN_POINT('Ctrl Pts',(-36.0215692694273,-3.7760202560004,-4.661283468199));
#28437=CARTESIAN_POINT('Ctrl Pts',(-36.0679888174549,-4.42965756005859,
-3.92328151360667));
#28438=CARTESIAN_POINT('Ctrl Pts',(-36.1144083654825,-5.08329486411676,
-3.18527955901436));
#28439=CARTESIAN_POINT('Ctrl Pts',(-36.1608279135102,-5.54849205649576,
-2.28037901315418));
#28440=CARTESIAN_POINT('Ctrl Pts',(-36.2072474615378,-5.76830243503646,
-1.31935247464221));
#28441=CARTESIAN_POINT('Ctrl Pts',(-36.2281232436235,-5.86715547772177,
-0.887159972796121));
#28442=CARTESIAN_POINT('Ctrl Pts',(-36.2489990257093,-5.91637958992632,
-0.443616115333533));
#28443=CARTESIAN_POINT('Ctrl Pts',(-36.2698748077951,-5.91625954349593,
-4.60302636559606E-5));
#28444=CARTESIAN_POINT('Ctrl Pts',(-36.5216251922048,-5.91632433790914,
-8.97973128488559E-5));
#28445=CARTESIAN_POINT('Ctrl Pts',(-36.5031884888862,-5.91653398030391,
-0.391821888062817));
#28446=CARTESIAN_POINT('Ctrl Pts',(-36.4847517855676,-5.87821607271003,
-0.783513512054098));
#28447=CARTESIAN_POINT('Ctrl Pts',(-36.4663150822489,-5.80096959006355,
-1.16737125606198));
#28448=CARTESIAN_POINT('Ctrl Pts',(-36.4198955342213,-5.60648000322127,
-2.1338402975065));
#28449=CARTESIAN_POINT('Ctrl Pts',(-36.3734759861937,-5.16521392348355,
-3.05064871239451));
#28450=CARTESIAN_POINT('Ctrl Pts',(-36.3270564381661,-4.53118854705755,
-3.80556621087274));
#28451=CARTESIAN_POINT('Ctrl Pts',(-36.2806368901385,-3.89716317063153,
-4.560483709351));
#28452=CARTESIAN_POINT('Ctrl Pts',(-36.2342173421109,-3.07037849751719,
-5.1535102914195));
#28453=CARTESIAN_POINT('Ctrl Pts',(-36.1877977940833,-2.15204464097599,
-5.51205113343194));
#28454=CARTESIAN_POINT('Ctrl Pts',(-36.1413782460557,-1.23371078443479,
-5.87059197544438));
#28455=CARTESIAN_POINT('Ctrl Pts',(-36.0949586980281,-0.223827744466776,
-5.99464707740077));
#28456=CARTESIAN_POINT('Ctrl Pts',(-36.0485391500005,0.75398054130614,-5.86903034390295));
#28457=CARTESIAN_POINT('Ctrl Pts',(-36.0021196019729,1.73178882707903,-5.74341361040513));
#28458=CARTESIAN_POINT('Ctrl Pts',(-35.9557000539452,2.67752235865676,-5.36812504145309));
#28459=CARTESIAN_POINT('Ctrl Pts',(-35.9092805059176,3.47541000365299,-4.78910525472458));
#28460=CARTESIAN_POINT('Ctrl Pts',(-35.86286095789,4.27329764864928,-4.21008546799603));
#28461=CARTESIAN_POINT('Ctrl Pts',(-35.8164414098624,4.92333940706406,-3.42733446349096));
#28462=CARTESIAN_POINT('Ctrl Pts',(-35.7700218618348,5.34596099295176,-2.53667201194006));
#28463=CARTESIAN_POINT('Ctrl Pts',(-35.7236023138072,5.76858257883944,-1.64600956038922));
#28464=CARTESIAN_POINT('Ctrl Pts',(-35.6771827657796,5.96378399220007,-0.647435661792543));
#28465=CARTESIAN_POINT('Ctrl Pts',(-35.6307632177519,5.9076698249577,0.336810144749435));
#28466=CARTESIAN_POINT('Ctrl Pts',(-35.5843436697243,5.85155565771532,1.32105595129147));
#28467=CARTESIAN_POINT('Ctrl Pts',(-35.5379241216967,5.54412590986989,2.29097366577883));
#28468=CARTESIAN_POINT('Ctrl Pts',(-35.4915045736691,5.02301432163358,3.12783167050048));
#28469=CARTESIAN_POINT('Ctrl Pts',(-35.4450850256415,4.50190273339729,3.96468967522209));
#28470=CARTESIAN_POINT('Ctrl Pts',(-35.3986654776139,3.76710930477012,4.66848797017802));
#28471=CARTESIAN_POINT('Ctrl Pts',(-35.3522459295863,2.90858312232014,5.15307171062816));
#28472=CARTESIAN_POINT('Ctrl Pts',(-35.3058263815587,2.05005693987014,5.6376554510783));
#28473=CARTESIAN_POINT('Ctrl Pts',(-35.2594068335311,1.0677980035973,5.90302463702264));
#28474=CARTESIAN_POINT('Ctrl Pts',(-35.2129872855034,0.08204867094368,5.91669433467018));
#28475=CARTESIAN_POINT('Ctrl Pts',(-35.1665677374758,-0.903700661709968,
5.93036403231773));
#28476=CARTESIAN_POINT('Ctrl Pts',(-35.1201481894482,-1.89294039074434,
5.69233424166847));
#28477=CARTESIAN_POINT('Ctrl Pts',(-35.0737286414206,-2.7645736111563,5.23174316865995));
#28478=CARTESIAN_POINT('Ctrl Pts',(-35.027309093393,-3.63620683156822,4.77115209565145));
#28479=CARTESIAN_POINT('Ctrl Pts',(-34.9808895453654,-4.39023354335769,
4.0879997402837));
#28480=CARTESIAN_POINT('Ctrl Pts',(-34.9344699973377,-4.93435023463825,
3.26591359289361));
#28481=CARTESIAN_POINT('Ctrl Pts',(-34.8880504493101,-5.47846692591882,
2.4438274455035));
#28482=CARTESIAN_POINT('Ctrl Pts',(-34.8416309012825,-5.81267359669049,
1.48280750609104));
#28483=CARTESIAN_POINT('Ctrl Pts',(-34.7952113532549,-5.89605863344435,
0.500496179114509));
#28484=CARTESIAN_POINT('Ctrl Pts',(-34.7873492995716,-5.91018151191266,
0.334122642218592));
#28485=CARTESIAN_POINT('Ctrl Pts',(-34.7794872458882,-5.91710931766303,
0.167138340296805));
#28486=CARTESIAN_POINT('Ctrl Pts',(-34.7716251922048,-5.91694163414713,
0.000140169273084226));
#28487=CARTESIAN_POINT('Origin',(-29.75,0.,0.));
#28488=CARTESIAN_POINT('',(-32.7698748077951,-5.91649785403418,-0.000138834737503368));
#28489=CARTESIAN_POINT('',(-33.0216251922048,-5.91664686417118,-0.000153939560766411));
#28490=CARTESIAN_POINT('',(-29.75,-5.91675,-7.2459289488551E-16));
#28491=CARTESIAN_POINT('Ctrl Pts',(-32.7698748077951,-5.91649785403418,
-0.000138834737503368));
#28492=CARTESIAN_POINT('Ctrl Pts',(-32.8015965397133,-5.91591751325044,
0.673809007249405));
#28493=CARTESIAN_POINT('Ctrl Pts',(-32.8333182716315,-5.80093975986991,
1.34794980680733));
#28494=CARTESIAN_POINT('Ctrl Pts',(-32.8650400035497,-5.57520380049187,
1.98270182260802));
#28495=CARTESIAN_POINT('Ctrl Pts',(-32.9114595515773,-5.24487627502982,
2.91155721294634));
#28496=CARTESIAN_POINT('Ctrl Pts',(-32.9578790996049,-4.67737645971137,
3.75606735812451));
#28497=CARTESIAN_POINT('Ctrl Pts',(-33.0042986476325,-3.9421743416468,4.41285229692244));
#28498=CARTESIAN_POINT('Ctrl Pts',(-33.0507181956601,-3.20697222358221,
5.0696372357204));
#28499=CARTESIAN_POINT('Ctrl Pts',(-33.0971377436877,-2.30406780277147,
5.53869696813813));
#28500=CARTESIAN_POINT('Ctrl Pts',(-33.1435572917153,-1.34398932395124,
5.7626119625997));
#28501=CARTESIAN_POINT('Ctrl Pts',(-33.1899768397429,-0.383910845131006,
5.98652695706128));
#28502=CARTESIAN_POINT('Ctrl Pts',(-33.2363963877706,0.633341691698729,
5.96529721356671));
#28503=CARTESIAN_POINT('Ctrl Pts',(-33.2828159357982,1.58324221848665,5.70152155235719));
#28504=CARTESIAN_POINT('Ctrl Pts',(-33.3292354838258,2.53314274527455,5.43774589114768));
#28505=CARTESIAN_POINT('Ctrl Pts',(-33.3756550318534,3.41569126202065,4.93142431222322));
#28506=CARTESIAN_POINT('Ctrl Pts',(-33.422074579881,4.12285137394988,4.24453772308737));
#28507=CARTESIAN_POINT('Ctrl Pts',(-33.4684941279086,4.83001148587914,3.55765113395147));
#28508=CARTESIAN_POINT('Ctrl Pts',(-33.5149136759362,5.36178319299148,2.69019953460422));
#28509=CARTESIAN_POINT('Ctrl Pts',(-33.5613332239639,5.65307013288908,1.74837124405247));
#28510=CARTESIAN_POINT('Ctrl Pts',(-33.6077527719915,5.94435707278667,0.806542953500733));
#28511=CARTESIAN_POINT('Ctrl Pts',(-33.6541723200191,5.99515924546949,-0.209662028255445));
#28512=CARTESIAN_POINT('Ctrl Pts',(-33.7005918680467,5.79925774797727,-1.175845868691));
#28513=CARTESIAN_POINT('Ctrl Pts',(-33.7470114160743,5.60335625048504,-2.14202970912655));
#28514=CARTESIAN_POINT('Ctrl Pts',(-33.7934309641019,5.16075108281776,-3.0581924082415));
#28515=CARTESIAN_POINT('Ctrl Pts',(-33.8398505121295,4.52562336444508,-3.81218272090687));
#28516=CARTESIAN_POINT('Ctrl Pts',(-33.8862700601571,3.89049564607243,-4.56617303357221));
#28517=CARTESIAN_POINT('Ctrl Pts',(-33.9326896081848,3.06284537699438,-5.15799095978799));
#28518=CARTESIAN_POINT('Ctrl Pts',(-33.9791091562124,2.14398863163539,-5.51518963244332));
#28519=CARTESIAN_POINT('Ctrl Pts',(-34.02552870424,1.22513188627637,-5.87238830509866));
#28520=CARTESIAN_POINT('Ctrl Pts',(-34.0719482522676,0.215068664636392,
-5.99496772419353));
#28521=CARTESIAN_POINT('Ctrl Pts',(-34.1183678002952,-0.762555038882753,
-5.86792243873985));
#28522=CARTESIAN_POINT('Ctrl Pts',(-34.1647873483228,-1.7401787424019,-5.74087715328617));
#28523=CARTESIAN_POINT('Ctrl Pts',(-34.2112068963505,-2.68536292780023,
-5.36420716328394));
#28524=CARTESIAN_POINT('Ctrl Pts',(-34.2576264443781,-3.48240371041724,
-4.78402219184488));
#28525=CARTESIAN_POINT('Ctrl Pts',(-34.3040459924057,-4.27944449303424,
-4.20383722040583));
#28526=CARTESIAN_POINT('Ctrl Pts',(-34.3504655404333,-4.92834187286995,
-3.42013726752995));
#28527=CARTESIAN_POINT('Ctrl Pts',(-34.3968850884609,-5.34966165206868,
-2.528858268622));
#28528=CARTESIAN_POINT('Ctrl Pts',(-34.4378816615723,-5.72176064624512,
-1.74170315415062));
#28529=CARTESIAN_POINT('Ctrl Pts',(-34.4788782346837,-5.91634964587558,
-0.870636636180083));
#28530=CARTESIAN_POINT('Ctrl Pts',(-34.5198748077951,-5.9170907741469,0.000109654298403733));
#28531=CARTESIAN_POINT('Ctrl Pts',(-34.7716251922048,-5.91694163414713,
0.000140169273084226));
#28532=CARTESIAN_POINT('Ctrl Pts',(-34.7330676978606,-5.91611927188961,
-0.818860984124561));
#28533=CARTESIAN_POINT('Ctrl Pts',(-34.6945102035163,-5.74463840154745,
-1.63819571286224));
#28534=CARTESIAN_POINT('Ctrl Pts',(-34.6559527091721,-5.41424544436451,
-2.38745682735834));
#28535=CARTESIAN_POINT('Ctrl Pts',(-34.6095331611445,-5.01648381579477,
-3.28949579231404));
#28536=CARTESIAN_POINT('Ctrl Pts',(-34.5631136131169,-4.38839715591919,
-4.0899710076849));
#28537=CARTESIAN_POINT('Ctrl Pts',(-34.5166940650892,-3.60687213674706,
-4.69089300916996));
#28538=CARTESIAN_POINT('Ctrl Pts',(-34.4702745170616,-2.82534711757491,
-5.29181501065503));
#28539=CARTESIAN_POINT('Ctrl Pts',(-34.423854969034,-1.8903837391062,-5.69318379825433));
#28540=CARTESIAN_POINT('Ctrl Pts',(-34.3774354210064,-0.916434714976281,
-5.84586616743047));
#28541=CARTESIAN_POINT('Ctrl Pts',(-34.3310158729788,0.0575143091536082,
-5.9985485366066));
#28542=CARTESIAN_POINT('Ctrl Pts',(-34.2845963249512,1.07044897894464,-5.90254448735958));
#28543=CARTESIAN_POINT('Ctrl Pts',(-34.2381767769236,1.99837179421368,-5.56960627032226));
#28544=CARTESIAN_POINT('Ctrl Pts',(-34.1917572288959,2.92629460948271,-5.23666805328494));
#28545=CARTESIAN_POINT('Ctrl Pts',(-34.1453376808684,3.76920557022969,-4.66679566845733));
#28546=CARTESIAN_POINT('Ctrl Pts',(-34.0989181328408,4.42392047797994,-3.92974953894413));
#28547=CARTESIAN_POINT('Ctrl Pts',(-34.0524985848131,5.0786353857302,-3.19270340943091));
#28548=CARTESIAN_POINT('Ctrl Pts',(-34.0060790367855,5.54515424048372,-2.28848353523204));
#28549=CARTESIAN_POINT('Ctrl Pts',(-33.9596594887579,5.76636854995267,-1.32777919114536));
#28550=CARTESIAN_POINT('Ctrl Pts',(-33.9132399407303,5.98758285942162,-0.36707484705867));
#28551=CARTESIAN_POINT('Ctrl Pts',(-33.8668203927027,5.96349262360604,0.650113966915861));
#28552=CARTESIAN_POINT('Ctrl Pts',(-33.820400844675,5.69704682738031,1.59926898330386));
#28553=CARTESIAN_POINT('Ctrl Pts',(-33.7739812966474,5.43060103115459,2.54842399969182));
#28554=CARTESIAN_POINT('Ctrl Pts',(-33.7275617486198,4.92179967451871,3.42954521849328));
#28555=CARTESIAN_POINT('Ctrl Pts',(-33.6811422005922,4.23292722476782,4.13477096634641));
#28556=CARTESIAN_POINT('Ctrl Pts',(-33.6347226525646,3.54405477501693,4.83999671419954));
#28557=CARTESIAN_POINT('Ctrl Pts',(-33.588303104537,2.67511123215103,5.36932699110438));
#28558=CARTESIAN_POINT('Ctrl Pts',(-33.5418835565094,1.73246755012107,5.65796430017894));
#28559=CARTESIAN_POINT('Ctrl Pts',(-33.4954640084818,0.789823868091082,
5.9466016092535));
#28560=CARTESIAN_POINT('Ctrl Pts',(-33.4490444604542,-0.226519953102918,
5.99454595049775));
#28561=CARTESIAN_POINT('Ctrl Pts',(-33.4026249124266,-1.19214908502915,
5.79592825985502));
#28562=CARTESIAN_POINT('Ctrl Pts',(-33.3562053643989,-2.15777821695538,
5.59731056921229));
#28563=CARTESIAN_POINT('Ctrl Pts',(-33.3097858163713,-3.07269265961378,
5.15213084668259));
#28564=CARTESIAN_POINT('Ctrl Pts',(-33.2633662683437,-3.82489397208368,
4.5148853735881));
#28565=CARTESIAN_POINT('Ctrl Pts',(-33.2169467203161,-4.57709528455356,
3.87763990049363));
#28566=CARTESIAN_POINT('Ctrl Pts',(-33.1705271722885,-5.16658346683494,
3.04832867683433));
#28567=CARTESIAN_POINT('Ctrl Pts',(-33.1241076242609,-5.52119684535653,
2.12847110131826));
#28568=CARTESIAN_POINT('Ctrl Pts',(-33.0899468135755,-5.78216191298198,
1.45153472796112));
#28569=CARTESIAN_POINT('Ctrl Pts',(-33.0557860028902,-5.91592585562199,
0.72556117549773));
#28570=CARTESIAN_POINT('Ctrl Pts',(-33.0216251922048,-5.91664686417118,
-0.000153939560766411));
#28571=CARTESIAN_POINT('Origin',(-29.75,0.,0.));
#28572=CARTESIAN_POINT('',(-31.0198748077951,-5.91669010006987,0.000155330332996806));
#28573=CARTESIAN_POINT('',(-31.2716251922048,-5.91653587213954,0.000144386273298953));
#28574=CARTESIAN_POINT('',(-29.75,-5.91675,-7.2459289488551E-16));
#28575=CARTESIAN_POINT('Ctrl Pts',(-31.0198748077951,-5.91669010006987,
0.000155330332996806));
#28576=CARTESIAN_POINT('Ctrl Pts',(-31.0314757486877,-5.91694033579073,
0.246601513478828));
#28577=CARTESIAN_POINT('Ctrl Pts',(-31.0430766895802,-5.9018335866036,0.493017226461263));
#28578=CARTESIAN_POINT('Ctrl Pts',(-31.0546776304728,-5.87112738637305,
0.737473489267511));
#28579=CARTESIAN_POINT('Ctrl Pts',(-31.1010971785004,-5.74826080602,1.71563115225999));
#28580=CARTESIAN_POINT('Ctrl Pts',(-31.147516726528,-5.37563318085241,2.66241628028925));
#28581=CARTESIAN_POINT('Ctrl Pts',(-31.1939362745556,-4.79885939147213,
3.46192901072102));
#28582=CARTESIAN_POINT('Ctrl Pts',(-31.2403558225832,-4.22208560209187,
4.26144174115277));
#28583=CARTESIAN_POINT('Ctrl Pts',(-31.2867753706108,-3.44116564849892,
4.91368207398704));
#28584=CARTESIAN_POINT('Ctrl Pts',(-31.3331949186384,-2.5516951549488,5.33880658673855));
#28585=CARTESIAN_POINT('Ctrl Pts',(-31.3796144666661,-1.66222466139868,
5.76393109949005));
#28586=CARTESIAN_POINT('Ctrl Pts',(-31.4260340146937,-0.66420362789138,
5.9619397921588));
#28587=CARTESIAN_POINT('Ctrl Pts',(-31.4724535627213,0.320196084962679,
5.90859360605945));
#28588=CARTESIAN_POINT('Ctrl Pts',(-31.5188731107489,1.30459579781674,5.85524741996011));
#28589=CARTESIAN_POINT('Ctrl Pts',(-31.5652926587765,2.27537419001756,5.55054635509267));
#28590=CARTESIAN_POINT('Ctrl Pts',(-31.6117122068041,3.11369428475438,5.03179012236004));
#28591=CARTESIAN_POINT('Ctrl Pts',(-31.6581317548318,3.95201437949117,4.51303388962741));
#28592=CARTESIAN_POINT('Ctrl Pts',(-31.7045513028594,4.65787617676397,3.78022248902961));
#28593=CARTESIAN_POINT('Ctrl Pts',(-31.750970850887,5.14487223002471,2.92306237892945));
#28594=CARTESIAN_POINT('Ctrl Pts',(-31.7973903989146,5.63186828328546,2.06590226882927));
#28595=CARTESIAN_POINT('Ctrl Pts',(-31.8438099469422,5.89999859253413,1.08439344922673));
#28596=CARTESIAN_POINT('Ctrl Pts',(-31.8902294949698,5.9164402235167,0.0986864526962545));
#28597=CARTESIAN_POINT('Ctrl Pts',(-31.9366490429974,5.93288185449926,-0.887020543834223));
#28598=CARTESIAN_POINT('Ctrl Pts',(-31.983068591025,5.69763480721572,-1.87692571729264));
#28599=CARTESIAN_POINT('Ctrl Pts',(-32.0294881390526,5.23949664053988,-2.74985070288613));
#28600=CARTESIAN_POINT('Ctrl Pts',(-32.0759076870803,4.78135847386406,-3.62277568847961));
#28601=CARTESIAN_POINT('Ctrl Pts',(-32.1223272351079,4.10032918779596,-4.37872048620816));
#28602=CARTESIAN_POINT('Ctrl Pts',(-32.1687467831355,3.27977637902512,-4.92514678339447));
#28603=CARTESIAN_POINT('Ctrl Pts',(-32.2151663311631,2.45922357025426,-5.4715730805808));
#28604=CARTESIAN_POINT('Ctrl Pts',(-32.2615858791907,1.49914723878067,-5.80848087722487));
#28605=CARTESIAN_POINT('Ctrl Pts',(-32.3080054272183,0.517074278132762,
-5.8946279038872));
#28606=CARTESIAN_POINT('Ctrl Pts',(-32.3544249752459,-0.464998682515144,
-5.98077493054954));
#28607=CARTESIAN_POINT('Ctrl Pts',(-32.4008445232736,-1.46906827233735,
-5.81616118723014));
#28608=CARTESIAN_POINT('Ctrl Pts',(-32.4472640713012,-2.37222220206094,
-5.42093771947633));
#28609=CARTESIAN_POINT('Ctrl Pts',(-32.4936836193288,-3.27537613178452,
-5.02571425172252));
#28610=CARTESIAN_POINT('Ctrl Pts',(-32.5401031673564,-4.07761440140948,
-4.39988105953429));
#28611=CARTESIAN_POINT('Ctrl Pts',(-32.586522715384,-4.68073172391043,-3.62004895867039));
#28612=CARTESIAN_POINT('Ctrl Pts',(-32.6329422634116,-5.28384904641137,
-2.8402168578065));
#28613=CARTESIAN_POINT('Ctrl Pts',(-32.6793618114392,-5.6878454217883,-1.90638584826694));
#28614=CARTESIAN_POINT('Ctrl Pts',(-32.7257813594668,-5.84326599167394,
-0.932870025747903));
#28615=CARTESIAN_POINT('Ctrl Pts',(-32.7404791755762,-5.89247678869508,
-0.624625823747457));
#28616=CARTESIAN_POINT('Ctrl Pts',(-32.7551769916857,-5.91676674673342,
-0.312403041320129));
#28617=CARTESIAN_POINT('Ctrl Pts',(-32.7698748077951,-5.91649785403418,
-0.000138834737503368));
#28618=CARTESIAN_POINT('Ctrl Pts',(-33.0216251922048,-5.91664686417118,
-0.000153939560766411));
#28619=CARTESIAN_POINT('Ctrl Pts',(-33.0093664548626,-5.9169056008419,-0.260579579419119));
#28620=CARTESIAN_POINT('Ctrl Pts',(-32.9971077175203,-5.90003159228609,
-0.52097193872601));
#28621=CARTESIAN_POINT('Ctrl Pts',(-32.984848980178,-5.86575487809614,-0.779052979208239));
#28622=CARTESIAN_POINT('Ctrl Pts',(-32.9384294321504,-5.7359609575523,-1.75631555684574));
#28623=CARTESIAN_POINT('Ctrl Pts',(-32.8920098841228,-5.35663454170278,
-2.70043678474785));
#28624=CARTESIAN_POINT('Ctrl Pts',(-32.8455903360952,-4.77421053767591,
-3.49584289925422));
#28625=CARTESIAN_POINT('Ctrl Pts',(-32.7991707880676,-4.19178653364904,
-4.29124901376059));
#28626=CARTESIAN_POINT('Ctrl Pts',(-32.75275124004,-3.40626494144485,-4.93794001487121));
#28627=CARTESIAN_POINT('Ctrl Pts',(-32.7063316920124,-2.51380469083249,
-5.35675179662735));
#28628=CARTESIAN_POINT('Ctrl Pts',(-32.6599121439847,-1.62134444022013,
-5.77556357838349));
#28629=CARTESIAN_POINT('Ctrl Pts',(-32.6134925959571,-0.621945531199624,
-5.9664961407851));
#28630=CARTESIAN_POINT('Ctrl Pts',(-32.5670730479295,0.362051504208375,
-5.90617664336433));
#28631=CARTESIAN_POINT('Ctrl Pts',(-32.5206534999019,1.34604853961635,-5.84585714594356));
#28632=CARTESIAN_POINT('Ctrl Pts',(-32.4742339518743,2.31464370141184,-5.53428558870041));
#28633=CARTESIAN_POINT('Ctrl Pts',(-32.4278144038467,3.14926727099989,-5.009602727775));
#28634=CARTESIAN_POINT('Ctrl Pts',(-32.3813948558191,3.98389084058799,-4.48491986684956));
#28635=CARTESIAN_POINT('Ctrl Pts',(-32.3349753077914,4.68454281796865,-3.7471257022418));
#28636=CARTESIAN_POINT('Ctrl Pts',(-32.2885557597638,5.16545351208018,-2.88653665295634));
#28637=CARTESIAN_POINT('Ctrl Pts',(-32.2421362117362,5.64636420619168,-2.02594760367094));
#28638=CARTESIAN_POINT('Ctrl Pts',(-32.1957166637086,5.9075336170341,-1.04256366970781));
#28639=CARTESIAN_POINT('Ctrl Pts',(-32.149297115681,5.91699092256471,-0.0567649241045975));
#28640=CARTESIAN_POINT('Ctrl Pts',(-32.1028775676534,5.92644822809533,0.929033821498671));
#28641=CARTESIAN_POINT('Ctrl Pts',(-32.0564580196258,5.68419342831414,1.91724737874199));
#28642=CARTESIAN_POINT('Ctrl Pts',(-32.0100384715982,5.21988192990835,2.78690446053288));
#28643=CARTESIAN_POINT('Ctrl Pts',(-31.9636189235706,4.75557043150258,3.65656154232375));
#28644=CARTESIAN_POINT('Ctrl Pts',(-31.9171993755429,4.06920223447221,4.40766214866215));
#28645=CARTESIAN_POINT('Ctrl Pts',(-31.8707798275153,3.24479849356221,4.94826096426798));
#28646=CARTESIAN_POINT('Ctrl Pts',(-31.8243602794877,2.42039475265223,5.48885977987379));
#28647=CARTESIAN_POINT('Ctrl Pts',(-31.7779407314601,1.4579554678626,5.81895680474706));
#28648=CARTESIAN_POINT('Ctrl Pts',(-31.7315211834325,0.475296791558483,
5.89814350404057));
#28649=CARTESIAN_POINT('Ctrl Pts',(-31.6851016354049,-0.507361884745695,
5.97733020333409));
#28650=CARTESIAN_POINT('Ctrl Pts',(-31.6386820873773,-1.51023995256432,
5.80560657704785));
#28651=CARTESIAN_POINT('Ctrl Pts',(-31.5922625393497,-2.41057098173501,
5.40399402075344));
#28652=CARTESIAN_POINT('Ctrl Pts',(-31.5458429913221,-3.31090201090567,
5.00238146445905));
#28653=CARTESIAN_POINT('Ctrl Pts',(-31.4994234432944,-4.10868600142836,
4.3708799781565));
#28654=CARTESIAN_POINT('Ctrl Pts',(-31.4530038952668,-4.70626293290763,
3.5867942568067));
#28655=CARTESIAN_POINT('Ctrl Pts',(-31.4065843472392,-5.30383986438691,
2.80270853545689));
#28656=CARTESIAN_POINT('Ctrl Pts',(-31.3601647992116,-5.7012097368228,1.86603857905981));
#28657=CARTESIAN_POINT('Ctrl Pts',(-31.313745251184,-5.84972886933474,0.891446010476035));
#28658=CARTESIAN_POINT('Ctrl Pts',(-31.2997052315243,-5.89464984829539,
0.596671515580249));
#28659=CARTESIAN_POINT('Ctrl Pts',(-31.2856652118645,-5.91680557048392,
0.298427800523953));
#28660=CARTESIAN_POINT('Ctrl Pts',(-31.2716251922048,-5.91653587213954,
0.000144386273298953));
#28661=CARTESIAN_POINT('Origin',(-29.75,0.,0.));
#28662=CARTESIAN_POINT('',(-29.2698748077951,-5.91689808548129,-0.00014569106262019));
#28663=CARTESIAN_POINT('',(-29.5216251922048,-5.91705311546107,-0.000119369217152434));
#28664=CARTESIAN_POINT('',(-29.75,-5.91675,-7.2459289488551E-16));
#28665=CARTESIAN_POINT('Ctrl Pts',(-29.2698748077951,-5.91689808548129,
-0.00014569106262019));
#28666=CARTESIAN_POINT('Ctrl Pts',(-29.3077745056896,-5.91607341121319,
0.804900279929208));
#28667=CARTESIAN_POINT('Ctrl Pts',(-29.3456742035842,-5.7505552877361,1.61027491020334));
#28668=CARTESIAN_POINT('Ctrl Pts',(-29.3835739014787,-5.43102511781527,
2.34903599462667));
#28669=CARTESIAN_POINT('Ctrl Pts',(-29.4299934495063,-5.03966458216716,
3.25387053274719));
#28670=CARTESIAN_POINT('Ctrl Pts',(-29.4764129975339,-4.41726519851383,
4.05877576500959));
#28671=CARTESIAN_POINT('Ctrl Pts',(-29.5228325455616,-3.64001743598446,
4.66521993052002));
#28672=CARTESIAN_POINT('Ctrl Pts',(-29.5692520935892,-2.86276967345511,
5.27166409603043));
#28673=CARTESIAN_POINT('Ctrl Pts',(-29.6156716416168,-1.93067353204981,
5.67964719478885));
#28674=CARTESIAN_POINT('Ctrl Pts',(-29.6620911896444,-0.957830735118941,
5.83922633721742));
#28675=CARTESIAN_POINT('Ctrl Pts',(-29.708510737672,0.0150120618118707,
5.99880547964598));
#28676=CARTESIAN_POINT('Ctrl Pts',(-29.7549302856996,1.02860151426824,5.90998066574465));
#28677=CARTESIAN_POINT('Ctrl Pts',(-29.8013498337272,1.95885996742694,5.58362530641197));
#28678=CARTESIAN_POINT('Ctrl Pts',(-29.8477693817548,2.88911842058573,5.25726994707927));
#28679=CARTESIAN_POINT('Ctrl Pts',(-29.8941889297825,3.73604587444693,4.69338404231518));
#28680=CARTESIAN_POINT('Ctrl Pts',(-29.9406084778101,4.39596645508967,3.96099518557123));
#28681=CARTESIAN_POINT('Ctrl Pts',(-29.9870280258377,5.05588703573237,3.22860632882733));
#28682=CARTESIAN_POINT('Ctrl Pts',(-30.0334475738653,5.52880074315668,2.3277145201035));
#28683=CARTESIAN_POINT('Ctrl Pts',(-30.0798671218929,5.75681626485063,1.36860163201104));
#28684=CARTESIAN_POINT('Ctrl Pts',(-30.1262866699205,5.9848317865446,0.409488743918518));
#28685=CARTESIAN_POINT('Ctrl Pts',(-30.1727062179481,5.96794912250825,-0.607845223542657));
#28686=CARTESIAN_POINT('Ctrl Pts',(-30.2191257659758,5.70823494910223,-1.55886423406273));
#28687=CARTESIAN_POINT('Ctrl Pts',(-30.2655453140034,5.44852077569622,-2.50988324458275));
#28688=CARTESIAN_POINT('Ctrl Pts',(-30.311964862031,4.94597509292055,-3.3945872981616));
#28689=CARTESIAN_POINT('Ctrl Pts',(-30.3583844100586,4.26211658529701,-4.10467613189253));
#28690=CARTESIAN_POINT('Ctrl Pts',(-30.4048039580862,3.57825807767347,-4.81476496562346));
#28691=CARTESIAN_POINT('Ctrl Pts',(-30.4512235061138,2.71308674520206,-5.35023857950647));
#28692=CARTESIAN_POINT('Ctrl Pts',(-30.4976430541414,1.77251177004035,-5.64554744550611));
#28693=CARTESIAN_POINT('Ctrl Pts',(-30.544062602169,0.83193679487858,-5.94085631150576));
#28694=CARTESIAN_POINT('Ctrl Pts',(-30.5904821501966,-0.184041822973492,
-5.996000429622));
#28695=CARTESIAN_POINT('Ctrl Pts',(-30.6369016982243,-1.15105396112758,
-5.8042293814911));
#28696=CARTESIAN_POINT('Ctrl Pts',(-30.6833212462519,-2.11806609928161,
-5.61245833336021));
#28697=CARTESIAN_POINT('Ctrl Pts',(-30.7297407942795,-3.03611175773765,
-5.17377211898222));
#28698=CARTESIAN_POINT('Ctrl Pts',(-30.7761603423071,-3.79280919056725,
-4.54187212263189));
#28699=CARTESIAN_POINT('Ctrl Pts',(-30.8225798903347,-4.54950662339687,
-3.90997212628154));
#28700=CARTESIAN_POINT('Ctrl Pts',(-30.8689994383623,-5.14485583060003,
-3.08485834795886));
#28701=CARTESIAN_POINT('Ctrl Pts',(-30.9154189863899,-5.50597766643234,
-2.16753635981969));
#28702=CARTESIAN_POINT('Ctrl Pts',(-30.950237593525,-5.77684974218483,-1.4794668873992));
#28703=CARTESIAN_POINT('Ctrl Pts',(-30.9850562006601,-5.91593905243186,
-0.739518538394789));
#28704=CARTESIAN_POINT('Ctrl Pts',(-31.0198748077951,-5.91669010006987,
0.000155330332996806));
#28705=CARTESIAN_POINT('Ctrl Pts',(-31.2716251922048,-5.91653587213954,
0.000144386273298953));
#28706=CARTESIAN_POINT('Ctrl Pts',(-31.2392456638369,-5.91591388546114,
-0.687766065954424));
#28707=CARTESIAN_POINT('Ctrl Pts',(-31.206866135469,-5.79601778419154,-1.37588766634103));
#28708=CARTESIAN_POINT('Ctrl Pts',(-31.1744866071011,-5.56101605193026,
-2.02215338302906));
#28709=CARTESIAN_POINT('Ctrl Pts',(-31.1280670590735,-5.22411570942588,
-2.94864502717984));
#28710=CARTESIAN_POINT('Ctrl Pts',(-31.0816475110459,-4.65064663182914,
-3.78911313471092));
#28711=CARTESIAN_POINT('Ctrl Pts',(-31.0352279630183,-3.91080952820358,
-4.44067254685975));
#28712=CARTESIAN_POINT('Ctrl Pts',(-30.9888084149907,-3.170972424578,-5.0922319590086));
#28713=CARTESIAN_POINT('Ctrl Pts',(-30.9423888669631,-2.26476729492359,
-5.55488267577518));
#28714=CARTESIAN_POINT('Ctrl Pts',(-30.8959693189355,-1.30312643732579,
-5.77198971955638));
#28715=CARTESIAN_POINT('Ctrl Pts',(-30.8495497709079,-0.341485579728019,
-5.98909676333757));
#28716=CARTESIAN_POINT('Ctrl Pts',(-30.8031302228802,0.675591005813218,
-5.96066013413337));
#28717=CARTESIAN_POINT('Ctrl Pts',(-30.7567106748526,1.62359879016756,-5.69016087671414));
#28718=CARTESIAN_POINT('Ctrl Pts',(-30.710291126825,2.57160657452198,-5.41966161929489));
#28719=CARTESIAN_POINT('Ctrl Pts',(-30.6638715787974,3.45054555768951,-4.90709973366061));
#28720=CARTESIAN_POINT('Ctrl Pts',(-30.6174520307698,4.15282120275032,-4.21522002893198));
#28721=CARTESIAN_POINT('Ctrl Pts',(-30.5710324827422,4.85509684781106,-3.5233403242034));
#28722=CARTESIAN_POINT('Ctrl Pts',(-30.5246129347146,5.38070915476503,-2.65214280038055));
#28723=CARTESIAN_POINT('Ctrl Pts',(-30.4781933866869,5.66531575872777,-1.70827433049633));
#28724=CARTESIAN_POINT('Ctrl Pts',(-30.4317738386593,5.9499223626905,-0.764405860612103));
#28725=CARTESIAN_POINT('Ctrl Pts',(-30.3853542906317,5.99352326366199,0.25213355533349));
#28726=CARTESIAN_POINT('Ctrl Pts',(-30.3389347426041,5.79078109597846,1.2169051453504));
#28727=CARTESIAN_POINT('Ctrl Pts',(-30.2925151945765,5.58803892829493,2.18167673536735));
#28728=CARTESIAN_POINT('Ctrl Pts',(-30.2460956465489,5.13895369195636,3.09468049945561));
#28729=CARTESIAN_POINT('Ctrl Pts',(-30.1996760985213,4.49849975829773,3.84415189071883));
#28730=CARTESIAN_POINT('Ctrl Pts',(-30.1532565504937,3.8580458246391,4.59362328198205));
#28731=CARTESIAN_POINT('Ctrl Pts',(-30.1068370024661,3.02622319366041,5.17956230042023));
#28732=CARTESIAN_POINT('Ctrl Pts',(-30.0604174544384,2.10485869577162,5.53024174020959));
#28733=CARTESIAN_POINT('Ctrl Pts',(-30.0139979064108,1.18349419788286,5.88092117999895));
#28734=CARTESIAN_POINT('Ctrl Pts',(-29.9675783583832,0.172587833084095,
5.9963410411395));
#28735=CARTESIAN_POINT('Ctrl Pts',(-29.9211588103556,-0.804111191600269,
5.86237230358709));
#28736=CARTESIAN_POINT('Ctrl Pts',(-29.874739262328,-1.78081021628463,5.72840356603468));
#28737=CARTESIAN_POINT('Ctrl Pts',(-29.8283197143004,-2.7233019008546,5.34504622978926));
#28738=CARTESIAN_POINT('Ctrl Pts',(-29.7819001662728,-3.51621196075299,
4.75922864352822));
#28739=CARTESIAN_POINT('Ctrl Pts',(-29.7354806182452,-4.30912202065143,
4.17341105726715));
#28740=CARTESIAN_POINT('Ctrl Pts',(-29.6890610702175,-4.95245045587837,
3.38513322099041));
#28741=CARTESIAN_POINT('Ctrl Pts',(-29.6426415221899,-5.36744478599853,
2.49089146764347));
#28742=CARTESIAN_POINT('Ctrl Pts',(-29.6023027455282,-5.72807655235332,
1.71379173482464));
#28743=CARTESIAN_POINT('Ctrl Pts',(-29.5619639688665,-5.91627768814128,
0.856671432896323));
#28744=CARTESIAN_POINT('Ctrl Pts',(-29.5216251922048,-5.91705311546107,
-0.000119369217152434));
#28745=CARTESIAN_POINT('Origin',(-29.75,0.,0.));
#28746=CARTESIAN_POINT('',(-27.5198748077951,-5.91634884690258,0.000100288842562468));
#28747=CARTESIAN_POINT('',(-27.7716251922048,-5.91627280920936,5.84495287493138E-5));
#28748=CARTESIAN_POINT('',(-29.75,-5.91675,-7.2459289488551E-16));
#28749=CARTESIAN_POINT('Ctrl Pts',(-27.5198748077951,-5.91634884690258,
0.000100288842562468));
#28750=CARTESIAN_POINT('Ctrl Pts',(-27.537653714664,-5.91657582580226,0.377851435059495));
#28751=CARTESIAN_POINT('Ctrl Pts',(-27.5554326215329,-5.88096092710108,
0.755560324906384));
#28752=CARTESIAN_POINT('Ctrl Pts',(-27.5732115284019,-5.80909502975842,
1.12624103531533));
#28753=CARTESIAN_POINT('Ctrl Pts',(-27.6196310764295,-5.62145793272878,
2.09406381354322));
#28754=CARTESIAN_POINT('Ctrl Pts',(-27.6660506244571,-5.18669868205167,
3.01397566782382));
#28755=CARTESIAN_POINT('Ctrl Pts',(-27.7124701724847,-4.55803794621954,
3.77336640352018));
#28756=CARTESIAN_POINT('Ctrl Pts',(-27.7588897205123,-3.92937721038742,
4.53275713921654));
#28757=CARTESIAN_POINT('Ctrl Pts',(-27.8053092685399,-3.10681498940029,
5.13162675632866));
#28758=CARTESIAN_POINT('Ctrl Pts',(-27.8517288165675,-2.19104450878334,
5.49666516125209));
#28759=CARTESIAN_POINT('Ctrl Pts',(-27.8981483645951,-1.27527402816635,
5.86170356617553));
#28760=CARTESIAN_POINT('Ctrl Pts',(-27.9445679126228,-0.266295287919555,
5.99291075891027));
#28761=CARTESIAN_POINT('Ctrl Pts',(-27.9909874606504,0.712378473384235,
5.87422512720195));
#28762=CARTESIAN_POINT('Ctrl Pts',(-28.037407008678,1.69105223468803,5.75553949549364));
#28763=CARTESIAN_POINT('Ctrl Pts',(-28.0838265567056,2.63942101704879,5.38696103934229));
#28764=CARTESIAN_POINT('Ctrl Pts',(-28.1302461047332,3.44139109619033,4.813608963912));
#28765=CARTESIAN_POINT('Ctrl Pts',(-28.1766656527608,4.24336117533185,4.24025688848174));
#28766=CARTESIAN_POINT('Ctrl Pts',(-28.2230852007884,4.89893255125415,3.46213119377257));
#28767=CARTESIAN_POINT('Ctrl Pts',(-28.269504748816,5.32785403478351,2.57448544731431));
#28768=CARTESIAN_POINT('Ctrl Pts',(-28.3159242968437,5.75677551831288,1.68683970085604));
#28769=CARTESIAN_POINT('Ctrl Pts',(-28.3623438448712,5.9590471094493,0.689673902648605));
#28770=CARTESIAN_POINT('Ctrl Pts',(-28.4087633928988,5.90990791056824,-0.294944779568952));
#28771=CARTESIAN_POINT('Ctrl Pts',(-28.4551829409265,5.86076871168719,-1.27956346178651));
#28772=CARTESIAN_POINT('Ctrl Pts',(-28.5016024889541,5.56021872278872,-2.25163502801417));
#28773=CARTESIAN_POINT('Ctrl Pts',(-28.5480220369817,5.04504950448862,-3.09216419868856));
#28774=CARTESIAN_POINT('Ctrl Pts',(-28.5944415850093,4.52988028618852,-3.93269336936294));
#28775=CARTESIAN_POINT('Ctrl Pts',(-28.6408611330369,3.80009183848674,-4.641680144484));
#28776=CARTESIAN_POINT('Ctrl Pts',(-28.6872806810645,2.94502056764569,-5.13233453610888));
#28777=CARTESIAN_POINT('Ctrl Pts',(-28.7337002290922,2.08994929680464,-5.62298892773375));
#28778=CARTESIAN_POINT('Ctrl Pts',(-28.7801197771198,1.10959520282435,-5.89531093586248));
#28779=CARTESIAN_POINT('Ctrl Pts',(-28.8265393251474,0.123967463565065,
-5.91596450313635));
#28780=CARTESIAN_POINT('Ctrl Pts',(-28.872958873175,-0.861660275694191,
-5.93661807041022));
#28781=CARTESIAN_POINT('Ctrl Pts',(-28.9193784212026,-1.85256166023243,
-5.70560319682918));
#28782=CARTESIAN_POINT('Ctrl Pts',(-28.9657979692302,-2.72743637495993,
-5.25119936347283));
#28783=CARTESIAN_POINT('Ctrl Pts',(-29.0122175172578,-3.60231108968744,
-4.79679553011648));
#28784=CARTESIAN_POINT('Ctrl Pts',(-29.0586370652854,-4.36115913460428,
-4.1190027369848));
#28785=CARTESIAN_POINT('Ctrl Pts',(-29.105056613313,-4.9110867986007,-3.30079238835192));
#28786=CARTESIAN_POINT('Ctrl Pts',(-29.1514761613407,-5.46101446259712,
-2.48258203971906));
#28787=CARTESIAN_POINT('Ctrl Pts',(-29.1978957093683,-5.80202174567313,
-1.52395413558503));
#28788=CARTESIAN_POINT('Ctrl Pts',(-29.2443152573959,-5.89236454338969,
-0.54225826152871));
#28789=CARTESIAN_POINT('Ctrl Pts',(-29.2528351075289,-5.90894607272058,
-0.362077667822123));
#28790=CARTESIAN_POINT('Ctrl Pts',(-29.261354957662,-5.91708347221425,-0.181119983843553));
#28791=CARTESIAN_POINT('Ctrl Pts',(-29.2698748077951,-5.91689808548129,
-0.00014569106262019));
#28792=CARTESIAN_POINT('Ctrl Pts',(-29.5216251922048,-5.91705311546107,
-0.000119369217152434));
#28793=CARTESIAN_POINT('Ctrl Pts',(-29.5155444208389,-5.91717000537774,
-0.129274227327039));
#28794=CARTESIAN_POINT('Ctrl Pts',(-29.509463649473,-5.91302795979075,-0.258421598105164));
#28795=CARTESIAN_POINT('Ctrl Pts',(-29.5033828781071,-5.90457561496714,
-0.38728625260564));
#28796=CARTESIAN_POINT('Ctrl Pts',(-29.4569633300795,-5.84005188880219,
-1.37101654909073));
#28797=CARTESIAN_POINT('Ctrl Pts',(-29.4105437820519,-5.52434421145891,
-2.33827147164377));
#28798=CARTESIAN_POINT('Ctrl Pts',(-29.3641242340242,-4.99609965855499,
-3.17064536586931));
#28799=CARTESIAN_POINT('Ctrl Pts',(-29.3177046859966,-4.46785510565111,
-4.0030192600948));
#28800=CARTESIAN_POINT('Ctrl Pts',(-29.271285137969,-3.72707367718662,-4.70051212599278));
#28801=CARTESIAN_POINT('Ctrl Pts',(-29.2248655899414,-2.86443747542453,
-5.17774099233492));
#28802=CARTESIAN_POINT('Ctrl Pts',(-29.1784460419138,-2.00180127366234,
-5.65496985867711));
#28803=CARTESIAN_POINT('Ctrl Pts',(-29.1320264938862,-1.01731029860253,
-5.91193472546341));
#28804=CARTESIAN_POINT('Ctrl Pts',(-29.0856069458586,-0.0314801407377438,
-5.91717946618666));
#28805=CARTESIAN_POINT('Ctrl Pts',(-29.0391873978309,0.954350017126954,
-5.92242420690991));
#28806=CARTESIAN_POINT('Ctrl Pts',(-28.9927678498033,1.9415193577966,-5.67594882157016));
#28807=CARTESIAN_POINT('Ctrl Pts',(-28.9463483017757,2.80918442102537,-5.20792537609653));
#28808=CARTESIAN_POINT('Ctrl Pts',(-28.8999287537481,3.67684948425417,-4.73990193062289));
#28809=CARTESIAN_POINT('Ctrl Pts',(-28.8535092057205,4.42501027004205,-4.05033042501536));
#28810=CARTESIAN_POINT('Ctrl Pts',(-28.8070896576929,4.9620813386371,-3.22362414420033));
#28811=CARTESIAN_POINT('Ctrl Pts',(-28.7606701096653,5.49915240723215,-2.3969178633853));
#28812=CARTESIAN_POINT('Ctrl Pts',(-28.7142505616377,5.82513375863435,-1.43307680736279));
#28813=CARTESIAN_POINT('Ctrl Pts',(-28.6678310136101,5.90012067451813,-0.450088725081483));
#28814=CARTESIAN_POINT('Ctrl Pts',(-28.6214114655824,5.97510759040192,0.532899357199769));
#28815=CARTESIAN_POINT('Ctrl Pts',(-28.5749919175548,5.7991000707673,1.53503446573988));
#28816=CARTESIAN_POINT('Ctrl Pts',(-28.5285723695272,5.39364392019479,2.43364111907807));
#28817=CARTESIAN_POINT('Ctrl Pts',(-28.4821528214996,4.98818776962226,3.33224777241634));
#28818=CARTESIAN_POINT('Ctrl Pts',(-28.435733273472,4.35328298811181,4.12732597055274));
#28819=CARTESIAN_POINT('Ctrl Pts',(-28.3893137254444,3.56665088199201,4.72154692026962));
#28820=CARTESIAN_POINT('Ctrl Pts',(-28.3428941774168,2.78001877587223,5.31576786998648));
#28821=CARTESIAN_POINT('Ctrl Pts',(-28.2964746293892,1.84165934514321,5.7091315712838));
#28822=CARTESIAN_POINT('Ctrl Pts',(-28.2500550813615,0.866441028168872,
5.8534847551717));
#28823=CARTESIAN_POINT('Ctrl Pts',(-28.2036355333339,-0.10877728880544,
5.99783793905961));
#28824=CARTESIAN_POINT('Ctrl Pts',(-28.1572159853063,-1.12085449202507,
5.89318060553806));
#28825=CARTESIAN_POINT('Ctrl Pts',(-28.1107964372787,-2.04589804731732,
5.55232428936793));
#28826=CARTESIAN_POINT('Ctrl Pts',(-28.0643768892511,-2.97094160260959,
5.21146797319779));
#28827=CARTESIAN_POINT('Ctrl Pts',(-28.0179573412235,-3.80895150997454,
4.63441267437906));
#28828=CARTESIAN_POINT('Ctrl Pts',(-27.9715377931959,-4.45734352904509,
3.89179810606892));
#28829=CARTESIAN_POINT('Ctrl Pts',(-27.9251182451682,-5.10573554811564,
3.14918353775878));
#28830=CARTESIAN_POINT('Ctrl Pts',(-27.8786986971406,-5.56450967889178,
2.24100969995723));
#28831=CARTESIAN_POINT('Ctrl Pts',(-27.832279149113,-5.77750549260991,1.27844988841335));
#28832=CARTESIAN_POINT('Ctrl Pts',(-27.812061163477,-5.87027559669915,0.859207968348168));
#28833=CARTESIAN_POINT('Ctrl Pts',(-27.7918431778409,-5.91642084319709,
0.429648871767775));
#28834=CARTESIAN_POINT('Ctrl Pts',(-27.7716251922048,-5.91627280920936,
5.84495287493138E-5));
#28835=CARTESIAN_POINT('Origin',(-29.75,0.,0.));
#28836=CARTESIAN_POINT('',(-25.7698748077951,-5.91722620641212,-5.21401381919917E-5));
#28837=CARTESIAN_POINT('',(-26.0216251922048,-5.91726316729143,2.21583349696063E-6));
#28838=CARTESIAN_POINT('',(-29.75,-5.91675,-7.2459289488551E-16));
#28839=CARTESIAN_POINT('Ctrl Pts',(-25.7698748077951,-5.91722620641212,
-5.21401381919917E-5));
#28840=CARTESIAN_POINT('Ctrl Pts',(-25.813952471666,-5.91679392379654,0.936072799262249));
#28841=CARTESIAN_POINT('Ctrl Pts',(-25.8580301355369,-5.69073137008731,
1.8723991018519));
#28842=CARTESIAN_POINT('Ctrl Pts',(-25.9021077994078,-5.26280619948913,
2.70497224403705));
#28843=CARTESIAN_POINT('Ctrl Pts',(-25.9485273474354,-4.81214499686768,
3.58178071268355));
#28844=CARTESIAN_POINT('Ctrl Pts',(-25.994946895463,-4.13760107317096,4.34351814822099));
#28845=CARTESIAN_POINT('Ctrl Pts',(-26.0413664434906,-3.3217481251996,4.89693713734667));
#28846=CARTESIAN_POINT('Ctrl Pts',(-26.0877859915183,-2.50589517722821,
5.45035612647238));
#28847=CARTESIAN_POINT('Ctrl Pts',(-26.1342055395458,-1.54873320498214,
5.79545666918634));
#28848=CARTESIAN_POINT('Ctrl Pts',(-26.1806250875735,-0.56743234328704,
5.88999358829735));
#28849=CARTESIAN_POINT('Ctrl Pts',(-26.2270446356011,0.413868518408088,
5.98453050740837));
#28850=CARTESIAN_POINT('Ctrl Pts',(-26.2734641836287,1.4193082695522,5.82850380291644));
#28851=CARTESIAN_POINT('Ctrl Pts',(-26.3198837316563,2.32580689378816,5.44101334561858));
#28852=CARTESIAN_POINT('Ctrl Pts',(-26.3663032796839,3.23230551802405,5.05352288832076));
#28853=CARTESIAN_POINT('Ctrl Pts',(-26.4127228277115,4.03986301535175,4.43456867821703));
#28854=CARTESIAN_POINT('Ctrl Pts',(-26.4591423757391,4.64962295019926,3.65991944656879));
#28855=CARTESIAN_POINT('Ctrl Pts',(-26.5055619237667,5.25938288504676,2.88527021492055));
#28856=CARTESIAN_POINT('Ctrl Pts',(-26.5519814717944,5.67134525741409,1.95492596172779));
#28857=CARTESIAN_POINT('Ctrl Pts',(-26.598401019822,5.83508005846991,0.982773954497618));
#28858=CARTESIAN_POINT('Ctrl Pts',(-26.6448205678496,5.99881485952574,0.0106219472674482));
#28859=CARTESIAN_POINT('Ctrl Pts',(-26.6912401158772,5.91432208927007,-1.00333781400015));
#28860=CARTESIAN_POINT('Ctrl Pts',(-26.7376596639048,5.59194485531658,-1.93498234345703));
#28861=CARTESIAN_POINT('Ctrl Pts',(-26.7840792119324,5.26956762136309,-2.86662687291391));
#28862=CARTESIAN_POINT('Ctrl Pts',(-26.83049875996,4.70930592371177,-3.7159561705601));
#28863=CARTESIAN_POINT('Ctrl Pts',(-26.8769183079876,3.97974370171135,-4.37900034289573));
#28864=CARTESIAN_POINT('Ctrl Pts',(-26.9233378560153,3.25018147971088,-5.0420445152314));
#28865=CARTESIAN_POINT('Ctrl Pts',(-26.9697574040429,2.35131873336127,-5.5188035622565));
#28866=CARTESIAN_POINT('Ctrl Pts',(-27.0161769520705,1.3931889494008,-5.75091544761872));
#28867=CARTESIAN_POINT('Ctrl Pts',(-27.0625965000981,0.435059165440296,
-5.98302733298095));
#28868=CARTESIAN_POINT('Ctrl Pts',(-27.1090160481257,-0.582337656131013,
-5.9704920566803));
#28869=CARTESIAN_POINT('Ctrl Pts',(-27.1554355961533,-1.53445778477314,
-5.71484411345937));
#28870=CARTESIAN_POINT('Ctrl Pts',(-27.2018551441809,-2.4865779134152,-5.45919617023846));
#28871=CARTESIAN_POINT('Ctrl Pts',(-27.2482746922086,-3.37342134912802,
-4.9604355600973));
#28872=CARTESIAN_POINT('Ctrl Pts',(-27.2946942402362,-4.08642593843634,
-4.27961762124454));
#28873=CARTESIAN_POINT('Ctrl Pts',(-27.3411137882638,-4.79943052774466,
-3.59879968239178));
#28874=CARTESIAN_POINT('Ctrl Pts',(-27.3875333362914,-5.33859627064848,
-2.73592441482741));
#28875=CARTESIAN_POINT('Ctrl Pts',(-27.433952884319,-5.63792167040933,-1.79661992995765));
#28876=CARTESIAN_POINT('Ctrl Pts',(-27.4625935254777,-5.82260402360958,
-1.21707351399728));
#28877=CARTESIAN_POINT('Ctrl Pts',(-27.4912341666364,-5.91598319893197,
-0.608431782664779));
#28878=CARTESIAN_POINT('Ctrl Pts',(-27.5198748077951,-5.91634884690258,
0.000100288842562468));
#28879=CARTESIAN_POINT('Ctrl Pts',(-27.7716251922048,-5.91627280920936,
5.84495287493138E-5));
#28880=CARTESIAN_POINT('Ctrl Pts',(-27.7454236298133,-5.91608096409504,
-0.556670616052406));
#28881=CARTESIAN_POINT('Ctrl Pts',(-27.7192220674217,-5.83813980461213,
-1.11345229290792));
#28882=CARTESIAN_POINT('Ctrl Pts',(-27.6930205050302,-5.68317102369272,
-1.64789895011231));
#28883=CARTESIAN_POINT('Ctrl Pts',(-27.6466009570026,-5.40862324439725,
-2.59474219180798));
#28884=CARTESIAN_POINT('Ctrl Pts',(-27.600181408975,-4.89231018914614,-3.47148288991311));
#28885=CARTESIAN_POINT('Ctrl Pts',(-27.5537618609474,-4.19743586316544,
-4.17079560862606));
#28886=CARTESIAN_POINT('Ctrl Pts',(-27.5073423129197,-3.50256153718475,
-4.87010832733899));
#28887=CARTESIAN_POINT('Ctrl Pts',(-27.4609227648921,-2.62912594047447,
-5.39199306665975));
#28888=CARTESIAN_POINT('Ctrl Pts',(-27.4145032168645,-1.68404991777717,
-5.67256376859322));
#28889=CARTESIAN_POINT('Ctrl Pts',(-27.3680836688369,-0.738973895079876,
-5.95313447052669));
#28890=CARTESIAN_POINT('Ctrl Pts',(-27.3216641208093,0.27774255360444,-5.99239113507287));
#28891=CARTESIAN_POINT('Ctrl Pts',(-27.2752445727817,1.24163898497985,-5.78552819242116));
#28892=CARTESIAN_POINT('Ctrl Pts',(-27.2288250247541,2.20553541635532,-5.57866524976944));
#28893=CARTESIAN_POINT('Ctrl Pts',(-27.1824054767265,3.11661183042188,-5.1256826999198));
#28894=CARTESIAN_POINT('Ctrl Pts',(-27.1359859286988,3.86333961512852,-4.48203200038782));
#28895=CARTESIAN_POINT('Ctrl Pts',(-27.0895663806712,4.61006739983517,-3.83838130085584));
#28896=CARTESIAN_POINT('Ctrl Pts',(-27.0431468326436,5.19244655518189,-3.00406245164152));
#28897=CARTESIAN_POINT('Ctrl Pts',(-26.996727284616,5.53918565283136,-2.0812078554986));
#28898=CARTESIAN_POINT('Ctrl Pts',(-26.9503077365884,5.88592475048081,-1.15835325935572));
#28899=CARTESIAN_POINT('Ctrl Pts',(-26.9038881885608,5.99702379043304,-0.14696291628425));
#28900=CARTESIAN_POINT('Ctrl Pts',(-26.8574686405332,5.85888268214156,0.829154720919783));
#28901=CARTESIAN_POINT('Ctrl Pts',(-26.8110490925056,5.72074157385008,1.80527235812382));
#28902=CARTESIAN_POINT('Ctrl Pts',(-26.7646295444779,5.3333603173149,2.74611728946041));
#28903=CARTESIAN_POINT('Ctrl Pts',(-26.7182099964503,4.74415984585059,3.53651681621066));
#28904=CARTESIAN_POINT('Ctrl Pts',(-26.6717904484227,4.15495937438626,4.32691634296093));
#28905=CARTESIAN_POINT('Ctrl Pts',(-26.6253709003951,3.3639396879928,4.96687046512485));
#28906=CARTESIAN_POINT('Ctrl Pts',(-26.5789513523675,2.46793276076853,5.37803976581127));
#28907=CARTESIAN_POINT('Ctrl Pts',(-26.5325318043399,1.57192583354425,5.78920906649768));
#28908=CARTESIAN_POINT('Ctrl Pts',(-26.4861122563123,0.570931665489247,
5.97159354570657));
#28909=CARTESIAN_POINT('Ctrl Pts',(-26.4396927082847,-0.412513929154647,
5.90286676900091));
#28910=CARTESIAN_POINT('Ctrl Pts',(-26.3932731602571,-1.39595952379854,
5.83413999229525));
#28911=CARTESIAN_POINT('Ctrl Pts',(-26.3468536122294,-2.36185654503133,
5.51430195967498));
#28912=CARTESIAN_POINT('Ctrl Pts',(-26.3004340642018,-3.19196556474444,
4.98250536053977));
#28913=CARTESIAN_POINT('Ctrl Pts',(-26.2540145161742,-4.02207458445755,
4.45070876140456));
#28914=CARTESIAN_POINT('Ctrl Pts',(-26.2075949681466,-4.71639560265107,
3.70695359575438));
#28915=CARTESIAN_POINT('Ctrl Pts',(-26.161175420119,-5.18993392702325,2.84228599325523));
#28916=CARTESIAN_POINT('Ctrl Pts',(-26.1146586774809,-5.66446375982073,
1.97580792438233));
#28917=CARTESIAN_POINT('Ctrl Pts',(-26.0681419348428,-5.91728509811654,
0.987910548273195));
#28918=CARTESIAN_POINT('Ctrl Pts',(-26.0216251922048,-5.91726313461423,
2.21569239827814E-6));
#28919=CARTESIAN_POINT('Origin',(-29.75,0.,0.));
#28920=CARTESIAN_POINT('',(-24.0198748077951,-5.91624086672945,-1.49279102093503E-5));
#28921=CARTESIAN_POINT('',(-24.2716251922048,-5.91627733888446,-6.20456869606399E-5));
#28922=CARTESIAN_POINT('',(-29.75,-5.91675,-7.2459289488551E-16));
#28923=CARTESIAN_POINT('Ctrl Pts',(-24.0198748077951,-5.91624086672945,
-1.49279102093503E-5));
#28924=CARTESIAN_POINT('Ctrl Pts',(-24.0438316806403,-5.91619635734186,
0.509026985967046));
#28925=CARTESIAN_POINT('Ctrl Pts',(-24.0677885534856,-5.85118645077979,
1.01808005821168));
#28926=CARTESIAN_POINT('Ctrl Pts',(-24.0917454263309,-5.72134892474527,
1.51002331627965));
#28927=CARTESIAN_POINT('Ctrl Pts',(-24.1381649743585,-5.46977187984169,
2.46322717732729));
#28928=CARTESIAN_POINT('Ctrl Pts',(-24.1845845223861,-4.97480544970528,
3.35219380141024));
#28929=CARTESIAN_POINT('Ctrl Pts',(-24.2310040704138,-4.29704051136091,
4.06810112682996));
#28930=CARTESIAN_POINT('Ctrl Pts',(-24.2774236184414,-3.61927557301662,
4.7840084522496));
#28931=CARTESIAN_POINT('Ctrl Pts',(-24.323843166469,-2.75871212646441,5.32685647900603));
#28932=CARTESIAN_POINT('Ctrl Pts',(-24.3702627144966,-1.82069528358946,
5.63019294684535));
#28933=CARTESIAN_POINT('Ctrl Pts',(-24.4166822625242,-0.882678440714442,
5.93352941468469));
#28934=CARTESIAN_POINT('Ctrl Pts',(-24.4631018105518,0.132791798483318,
5.99735432360688));
#28935=CARTESIAN_POINT('Ctrl Pts',(-24.5095213585794,1.10140754433813,5.8138546039325));
#28936=CARTESIAN_POINT('Ctrl Pts',(-24.555940906607,2.07002329019295,5.63035488425812));
#28937=CARTESIAN_POINT('Ctrl Pts',(-24.6023604546346,2.9917845427048,5.19953053598718));
#28938=CARTESIAN_POINT('Ctrl Pts',(-24.6487800026623,3.75385471479075,4.57412054002027));
#28939=CARTESIAN_POINT('Ctrl Pts',(-24.6951995506899,4.51592488687675,3.94871054405332));
#28940=CARTESIAN_POINT('Ctrl Pts',(-24.7416190987175,5.11830397853682,3.12871490039038));
#28941=CARTESIAN_POINT('Ctrl Pts',(-24.7880386467451,5.48725228694898,2.21451264926738));
#28942=CARTESIAN_POINT('Ctrl Pts',(-24.8344581947727,5.85620059536113,1.3003103981444));
#28943=CARTESIAN_POINT('Ctrl Pts',(-24.8808777428003,5.99171812052539,0.291901539561299));
#28944=CARTESIAN_POINT('Ctrl Pts',(-24.9272972908279,5.87721560466181,-0.68727044946791));
#28945=CARTESIAN_POINT('Ctrl Pts',(-24.9737168388556,5.76271308879823,-1.66644243849709));
#28946=CARTESIAN_POINT('Ctrl Pts',(-25.0201363868831,5.39819053190684,-2.61637755797244));
#28947=CARTESIAN_POINT('Ctrl Pts',(-25.0665559349108,4.82827063983722,-3.42079034184762));
#28948=CARTESIAN_POINT('Ctrl Pts',(-25.1129754829384,4.2583507477676,-4.22520312572279));
#28949=CARTESIAN_POINT('Ctrl Pts',(-25.159395030966,3.48303352051976,-4.88409357399777));
#28950=CARTESIAN_POINT('Ctrl Pts',(-25.2058145789936,2.59722872956742,-5.31680419619734));
#28951=CARTESIAN_POINT('Ctrl Pts',(-25.2522341270212,1.71142393861504,-5.74951481839694));
#28952=CARTESIAN_POINT('Ctrl Pts',(-25.2986536750488,0.715131583958168,
-5.95604561452111));
#28953=CARTESIAN_POINT('Ctrl Pts',(-25.3450732230764,-0.269688088482717,
-5.91111430014025));
#28954=CARTESIAN_POINT('Ctrl Pts',(-25.391492771104,-1.25450776092355,-5.8661829857594));
#28955=CARTESIAN_POINT('Ctrl Pts',(-25.4379123191317,-2.22785475114838,
-5.56978956087356));
#28956=CARTESIAN_POINT('Ctrl Pts',(-25.4843318671593,-3.07057764969502,
-5.05821676399751));
#28957=CARTESIAN_POINT('Ctrl Pts',(-25.5307514151869,-3.91330054824167,
-4.54664396712146));
#28958=CARTESIAN_POINT('Ctrl Pts',(-25.5771709632145,-4.62539935511013,
-3.8198917982552));
#28959=CARTESIAN_POINT('Ctrl Pts',(-25.6235905112421,-5.11970312574842,
-2.96692498027738));
#28960=CARTESIAN_POINT('Ctrl Pts',(-25.6700100592697,-5.61400689638677,
-2.11395816229946));
#28961=CARTESIAN_POINT('Ctrl Pts',(-25.7164296072974,-5.89051563079491,
-1.13477669520995));
#28962=CARTESIAN_POINT('Ctrl Pts',(-25.762849155325,-5.91538075722584,-0.149246210787353));
#28963=CARTESIAN_POINT('Ctrl Pts',(-25.7651910394817,-5.91663521247405,
-0.099525816567977));
#28964=CARTESIAN_POINT('Ctrl Pts',(-25.7675329236384,-5.91724917395894,
-0.0497892625659706));
#28965=CARTESIAN_POINT('Ctrl Pts',(-25.7698748077951,-5.91722620641212,
-5.21401381919917E-5));
#28966=CARTESIAN_POINT('Ctrl Pts',(-26.0216251922048,-5.91726313461423,
2.21569239827814E-6));
#28967=CARTESIAN_POINT('Ctrl Pts',(-25.9753028387876,-5.91724126289539,
-0.983777738154382));
#28968=CARTESIAN_POINT('Ctrl Pts',(-25.9289804853705,-5.66661285648345,
-1.96756842312595));
#28969=CARTESIAN_POINT('Ctrl Pts',(-25.8826581319533,-5.19587372555123,
-2.83141308580155));
#28970=CARTESIAN_POINT('Ctrl Pts',(-25.8362385839257,-4.72414687911932,
-3.69707028690149));
#28971=CARTESIAN_POINT('Ctrl Pts',(-25.7898190358981,-4.03138465651247,
-4.44227759072061));
#28972=CARTESIAN_POINT('Ctrl Pts',(-25.7433994878705,-3.20239093145171,
-4.9758111053855));
#28973=CARTESIAN_POINT('Ctrl Pts',(-25.6969799398429,-2.37339720639091,
-5.50934462005042));
#28974=CARTESIAN_POINT('Ctrl Pts',(-25.6505603918153,-1.40817197887618,
-5.8312043455611));
#28975=CARTESIAN_POINT('Ctrl Pts',(-25.6041408437876,-0.424872439983136,
-5.90199010877387));
#28976=CARTESIAN_POINT('Ctrl Pts',(-25.55772129576,0.55842709890991,-5.97277587198664));
#28977=CARTESIAN_POINT('Ctrl Pts',(-25.5113017477324,1.55980094918128,-5.79248767290151));
#28978=CARTESIAN_POINT('Ctrl Pts',(-25.4648821997048,2.45666681812683,-5.3831953316814));
#28979=CARTESIAN_POINT('Ctrl Pts',(-25.4184626516772,3.35353268707233,-4.97390299046132));
#28980=CARTESIAN_POINT('Ctrl Pts',(-25.3720431036496,4.14589057469203,-4.3356065071063));
#28981=CARTESIAN_POINT('Ctrl Pts',(-25.325623555622,4.73674469217009,-3.54644238012129));
#28982=CARTESIAN_POINT('Ctrl Pts',(-25.2792040075944,5.32759880964815,-2.75727825313629));
#28983=CARTESIAN_POINT('Ctrl Pts',(-25.2327844595667,5.71694915698457,-1.8172464825213));
#28984=CARTESIAN_POINT('Ctrl Pts',(-25.1863649115391,5.85713375635887,-0.841420224645929));
#28985=CARTESIAN_POINT('Ctrl Pts',(-25.1399453635115,5.99731835573319,0.134406033229496));
#28986=CARTESIAN_POINT('Ctrl Pts',(-25.0935258154839,5.88833720714536,1.14602677836531));
#28987=CARTESIAN_POINT('Ctrl Pts',(-25.0471062674563,5.54353114134686,2.06960535350088));
#28988=CARTESIAN_POINT('Ctrl Pts',(-25.0006867194287,5.19872507554837,2.9931839286364));
#28989=CARTESIAN_POINT('Ctrl Pts',(-24.9542671714011,4.61809409253925,3.82872033377169));
#28990=CARTESIAN_POINT('Ctrl Pts',(-24.9078476233735,3.8727156196889,4.47393312012366));
#28991=CARTESIAN_POINT('Ctrl Pts',(-24.8614280753458,3.12733714683856,5.11914590647564));
#28992=CARTESIAN_POINT('Ctrl Pts',(-24.8150085273182,2.21721118414701,5.5740350740443));
#28993=CARTESIAN_POINT('Ctrl Pts',(-24.7685889792906,1.25374999500223,5.78291576839519));
#28994=CARTESIAN_POINT('Ctrl Pts',(-24.722169431263,0.290288805857399,5.99179646274609));
#28995=CARTESIAN_POINT('Ctrl Pts',(-24.6757498832354,-0.726507609740667,
5.9546686838792));
#28996=CARTESIAN_POINT('Ctrl Pts',(-24.6293303352078,-1.67216901941713,
5.67607739595078));
#28997=CARTESIAN_POINT('Ctrl Pts',(-24.5829107871802,-2.61783042909354,
5.39748610802238));
#28998=CARTESIAN_POINT('Ctrl Pts',(-24.5364912391526,-3.49235683284836,
4.87743131103248));
#28999=CARTESIAN_POINT('Ctrl Pts',(-24.4900716911249,-4.18869385576106,
4.17957505220703));
#29000=CARTESIAN_POINT('Ctrl Pts',(-24.4436521430973,-4.88503087867377,
3.48171879338158));
#29001=CARTESIAN_POINT('Ctrl Pts',(-24.3972325950697,-5.40317852074435,
2.60606107272057));
#29002=CARTESIAN_POINT('Ctrl Pts',(-24.3508130470421,-5.67970819742667,
1.6597947543013));
#29003=CARTESIAN_POINT('Ctrl Pts',(-24.3244170954297,-5.83695367428408,
1.12171110172871));
#29004=CARTESIAN_POINT('Ctrl Pts',(-24.2980211438172,-5.91607198801577,
0.560796160819298));
#29005=CARTESIAN_POINT('Ctrl Pts',(-24.2716251922048,-5.91627733888446,
-6.20456869606399E-5));
#29006=CARTESIAN_POINT('Origin',(-29.75,0.,0.));
#29007=CARTESIAN_POINT('',(-22.2698748077951,-5.91717032569028,8.22304250084477E-5));
#29008=CARTESIAN_POINT('',(-22.5216251922048,-5.91704156442688,0.000122038191318572));
#29009=CARTESIAN_POINT('',(-29.75,-5.91675,-7.2459289488551E-16));
#29010=CARTESIAN_POINT('Ctrl Pts',(-22.2698748077951,-5.91717032569028,
8.22304250084477E-5));
#29011=CARTESIAN_POINT('Ctrl Pts',(-22.2737108896147,-5.91722571336033,
0.0815554764548256));
#29012=CARTESIAN_POINT('Ctrl Pts',(-22.2775469714344,-5.91557804319747,
0.163026480149979));
#29013=CARTESIAN_POINT('Ctrl Pts',(-22.281383053254,-5.91221275274682,0.244426472890983));
#29014=CARTESIAN_POINT('Ctrl Pts',(-22.3278026012816,-5.87149014331214,
1.22942915274484));
#29015=CARTESIAN_POINT('Ctrl Pts',(-22.3742221493092,-5.57925869458383,
2.20403379364773));
#29016=CARTESIAN_POINT('Ctrl Pts',(-22.4206416973368,-5.0712916604527,3.04893503194394));
#29017=CARTESIAN_POINT('Ctrl Pts',(-22.4670612453645,-4.56332462632153,
3.89383627024019));
#29018=CARTESIAN_POINT('Ctrl Pts',(-22.5134807933921,-3.83962200678752,
4.60903410592975));
#29019=CARTESIAN_POINT('Ctrl Pts',(-22.5599003414197,-2.98877521684958,
5.1069782295931));
#29020=CARTESIAN_POINT('Ctrl Pts',(-22.6063198894473,-2.13792842691164,
5.60492235325644));
#29021=CARTESIAN_POINT('Ctrl Pts',(-22.6527394374749,-1.15993746656978,
5.88561276489358));
#29022=CARTESIAN_POINT('Ctrl Pts',(-22.6991589855025,-0.174522232773706,
5.91468899644434));
#29023=CARTESIAN_POINT('Ctrl Pts',(-22.7455785335302,0.810893001022308,
5.94376522799509));
#29024=CARTESIAN_POINT('Ctrl Pts',(-22.7919980815578,1.80373250827253,5.72122727945949));
#29025=CARTESIAN_POINT('Ctrl Pts',(-22.8384176295854,2.68245872031269,5.27431693664786));
#29026=CARTESIAN_POINT('Ctrl Pts',(-22.884837177613,3.56118493235285,4.82740659383624));
#29027=CARTESIAN_POINT('Ctrl Pts',(-22.9312567256406,4.32579784918294,4.1561238567486));
#29028=CARTESIAN_POINT('Ctrl Pts',(-22.9776762736682,4.88269805800541,3.34264320691608));
#29029=CARTESIAN_POINT('Ctrl Pts',(-23.0240958216958,5.43959826682792,2.52916255708353));
#29030=CARTESIAN_POINT('Ctrl Pts',(-23.0705153697234,5.7887857676428,1.57348399450608));
#29031=CARTESIAN_POINT('Ctrl Pts',(-23.1169349177511,5.88751508190382,0.592596063729021));
#29032=CARTESIAN_POINT('Ctrl Pts',(-23.1633544657787,5.98624439616484,-0.388291867047986));
#29033=CARTESIAN_POINT('Ctrl Pts',(-23.2097740138063,5.83451552387203,-1.39438916602461));
#29034=CARTESIAN_POINT('Ctrl Pts',(-23.2561935618339,5.45090222050147,-2.30253532370825));
#29035=CARTESIAN_POINT('Ctrl Pts',(-23.3026131098615,5.0672889171309,-3.2106814813919));
#29036=CARTESIAN_POINT('Ctrl Pts',(-23.3490326578891,4.45179118268257,-4.02087649778257));
#29037=CARTESIAN_POINT('Ctrl Pts',(-23.3954522059167,3.67975462701281,-4.63394106774891));
#29038=CARTESIAN_POINT('Ctrl Pts',(-23.4418717539443,2.907718071343,-5.24700563771528));
#29039=CARTESIAN_POINT('Ctrl Pts',(-23.4882913019719,1.97914269445174,-5.66293976125731));
#29040=CARTESIAN_POINT('Ctrl Pts',(-23.5347108499996,1.00769922842084,-5.83082723114243));
#29041=CARTESIAN_POINT('Ctrl Pts',(-23.5811303980272,0.0362557623899958,
-5.99871470102755));
#29042=CARTESIAN_POINT('Ctrl Pts',(-23.6275499460548,-0.978055792780479,
-5.9185555172558));
#29043=CARTESIAN_POINT('Ctrl Pts',(-23.6739694940824,-1.91106938670352,
-5.60016229529079));
#29044=CARTESIAN_POINT('Ctrl Pts',(-23.72038904211,-2.84408298062656,-5.28176907332579));
#29045=CARTESIAN_POINT('Ctrl Pts',(-23.7668085901376,-3.69579861330217,
-4.72514181316754));
#29046=CARTESIAN_POINT('Ctrl Pts',(-23.8132281381652,-4.36195427014207,
-3.99841954771901));
#29047=CARTESIAN_POINT('Ctrl Pts',(-23.8596476861928,-5.028109926982,-3.27169728227043));
#29048=CARTESIAN_POINT('Ctrl Pts',(-23.9060672342205,-5.5087056079862,-2.37488001153154));
#29049=CARTESIAN_POINT('Ctrl Pts',(-23.9524867822481,-5.74490961865291,
-1.41775082715593));
#29050=CARTESIAN_POINT('Ctrl Pts',(-23.9749494574304,-5.85921004150957,
-0.954590738579167));
#29051=CARTESIAN_POINT('Ctrl Pts',(-23.9974121326127,-5.91628260005259,
-0.477307738180849));
#29052=CARTESIAN_POINT('Ctrl Pts',(-24.0198748077951,-5.91624086672945,
-1.49279102093503E-5));
#29053=CARTESIAN_POINT('Ctrl Pts',(-24.2716251922048,-5.91627733888446,
-6.20456869606399E-5));
#29054=CARTESIAN_POINT('Ctrl Pts',(-24.2516015957896,-5.91643311515571,
-0.425521166771968));
#29055=CARTESIAN_POINT('Ctrl Pts',(-24.2315779993744,-5.87117822566273,
-0.850947639899966));
#29056=CARTESIAN_POINT('Ctrl Pts',(-24.2115544029593,-5.78016964510108,
-1.26635015227775));
#29057=CARTESIAN_POINT('Ctrl Pts',(-24.1651348549317,-5.56918970479912,
-2.22935382425988));
#29058=CARTESIAN_POINT('Ctrl Pts',(-24.118715306904,-5.11231811290117,-3.13848625204656));
#29059=CARTESIAN_POINT('Ctrl Pts',(-24.0722957588764,-4.46548240055963,
-3.88245679494493));
#29060=CARTESIAN_POINT('Ctrl Pts',(-24.0258762108488,-3.81864668821811,
-4.62642733784326));
#29061=CARTESIAN_POINT('Ctrl Pts',(-23.9794566628212,-2.98184685543302,
-5.20523599585329));
#29062=CARTESIAN_POINT('Ctrl Pts',(-23.9330371147936,-2.05751901236383,
-5.54802841990587));
#29063=CARTESIAN_POINT('Ctrl Pts',(-23.886617566766,-1.13319116929464,-5.89082084395845));
#29064=CARTESIAN_POINT('Ctrl Pts',(-23.8401980187383,-0.121335315941354,
-5.99759703405356));
#29065=CARTESIAN_POINT('Ctrl Pts',(-23.7937784707107,0.854183109871268,
-5.85528607748012));
#29066=CARTESIAN_POINT('Ctrl Pts',(-23.7473589226831,1.82970153568389,-5.71297512090667));
#29067=CARTESIAN_POINT('Ctrl Pts',(-23.7009393746556,2.76888253395585,-5.32157701766468));
#29068=CARTESIAN_POINT('Ctrl Pts',(-23.6545198266279,3.55675709486016,-4.72900441979956));
#29069=CARTESIAN_POINT('Ctrl Pts',(-23.6081002786003,4.34463165576448,-4.13643182193444));
#29070=CARTESIAN_POINT('Ctrl Pts',(-23.5616807305727,4.98119977930114,-3.3426847294462));
#29071=CARTESIAN_POINT('Ctrl Pts',(-23.515261182545,5.38853654260112,-2.44492898943387));
#29072=CARTESIAN_POINT('Ctrl Pts',(-23.4688416345174,5.79587330590112,-1.54717324942149));
#29073=CARTESIAN_POINT('Ctrl Pts',(-23.4224220864899,5.97397870896441,-0.545408861885016));
#29074=CARTESIAN_POINT('Ctrl Pts',(-23.3760025384623,5.90105013666917,0.437734073198114));
#29075=CARTESIAN_POINT('Ctrl Pts',(-23.3295829904347,5.82812156437394,1.42087700828124));
#29076=CARTESIAN_POINT('Ctrl Pts',(-23.283163442407,5.50415901672018,2.38539849091103));
#29077=CARTESIAN_POINT('Ctrl Pts',(-23.2367438943794,4.96882008196121,3.21322747831846));
#29078=CARTESIAN_POINT('Ctrl Pts',(-23.1903243463518,4.43348114720223,4.0410564657259));
#29079=CARTESIAN_POINT('Ctrl Pts',(-23.1439047983242,3.68676582533804,4.73219295791099));
#29080=CARTESIAN_POINT('Ctrl Pts',(-23.0974852502966,2.82008261093496,5.20203209350194));
#29081=CARTESIAN_POINT('Ctrl Pts',(-23.051065702269,1.95339939653199,5.67187122909283));
#29082=CARTESIAN_POINT('Ctrl Pts',(-23.0046461542413,0.966748289590168,
5.92041300808964));
#29083=CARTESIAN_POINT('Ctrl Pts',(-22.9582266062137,-0.0190906887673131,
5.91723240881446));
#29084=CARTESIAN_POINT('Ctrl Pts',(-22.9118070581861,-1.00492966712491,
5.91405180953929));
#29085=CARTESIAN_POINT('Ctrl Pts',(-22.8653875101585,-1.98995651689816,
5.65914883199208));
#29086=CARTESIAN_POINT('Ctrl Pts',(-22.8189679621309,-2.85359004896614,
5.18372719833551));
#29087=CARTESIAN_POINT('Ctrl Pts',(-22.7725484141033,-3.71722358103407,
4.70830556467896));
#29088=CARTESIAN_POINT('Ctrl Pts',(-22.7261288660757,-4.45946379539674,
4.01236527491309));
#29089=CARTESIAN_POINT('Ctrl Pts',(-22.679709318048,-4.98945001380782,3.18109924303455));
#29090=CARTESIAN_POINT('Ctrl Pts',(-22.6332897700204,-5.51943623221891,
2.349833211156));
#29091=CARTESIAN_POINT('Ctrl Pts',(-22.5868702219928,-5.83716845467843,
1.38324143716479));
#29092=CARTESIAN_POINT('Ctrl Pts',(-22.5404506739652,-5.90375177267192,
0.399648396712717));
#29093=CARTESIAN_POINT('Ctrl Pts',(-22.5341755133784,-5.91275274382662,
0.26668277030843));
#29094=CARTESIAN_POINT('Ctrl Pts',(-22.5279003527916,-5.91716406927873,
0.13340645256461));
#29095=CARTESIAN_POINT('Ctrl Pts',(-22.5216251922048,-5.91704156442688,
0.000122038191318572));
#29096=CARTESIAN_POINT('Origin',(-29.75,0.,0.));
#29097=CARTESIAN_POINT('',(-20.5198748077951,-5.91641453668928,-0.000121371007781868));
#29098=CARTESIAN_POINT('',(-20.7716251922048,-5.9165474513811,-0.000145824772724381));
#29099=CARTESIAN_POINT('',(-29.75,-5.91675,-7.2459289488551E-16));
#29100=CARTESIAN_POINT('Ctrl Pts',(-20.5198748077951,-5.91641453668928,
-0.000121371007781868));
#29101=CARTESIAN_POINT('Ctrl Pts',(-20.5500096466167,-5.91594204778621,
0.640137786987893));
#29102=CARTESIAN_POINT('Ctrl Pts',(-20.5801444854383,-5.81238320478607,
1.28054610164413));
#29103=CARTESIAN_POINT('Ctrl Pts',(-20.61027932426,-5.60827747628413,1.88712153381709));
#29104=CARTESIAN_POINT('Ctrl Pts',(-20.6566988722876,-5.29387408016884,
2.82148715537517));
#29105=CARTESIAN_POINT('Ctrl Pts',(-20.7031184203152,-4.74089142151915,
3.67557357075011));
#29106=CARTESIAN_POINT('Ctrl Pts',(-20.7495379683428,-4.01702238257332,
4.34482854808991));
#29107=CARTESIAN_POINT('Ctrl Pts',(-20.7959575163704,-3.2931533436275,5.0140835254297));
#29108=CARTESIAN_POINT('Ctrl Pts',(-20.842377064398,-2.39839792438554,5.49850706473436));
#29109=CARTESIAN_POINT('Ctrl Pts',(-20.8887966124256,-1.44228681677674,
5.73879888761961));
#29110=CARTESIAN_POINT('Ctrl Pts',(-20.9352161604533,-0.486175709167936,
5.97909071050486));
#29111=CARTESIAN_POINT('Ctrl Pts',(-20.9816357084809,0.531291086807709,
5.97525081697072));
#29112=CARTESIAN_POINT('Ctrl Pts',(-21.0280552565085,1.48556127475539,5.72774926418216));
#29113=CARTESIAN_POINT('Ctrl Pts',(-21.0744748045361,2.43983146270312,5.48024771139358));
#29114=CARTESIAN_POINT('Ctrl Pts',(-21.1208943525637,3.33090504262288,4.98908449935057));
#29115=CARTESIAN_POINT('Ctrl Pts',(-21.1673139005913,4.04970203168403,4.31438493750457));
#29116=CARTESIAN_POINT('Ctrl Pts',(-21.2137334486189,4.76849902074518,3.63968537565857));
#29117=CARTESIAN_POINT('Ctrl Pts',(-21.2601529966465,5.31501941894773,2.78144946400959));
#29118=CARTESIAN_POINT('Ctrl Pts',(-21.3065725446742,5.62236141594072,1.84473739131974));
#29119=CARTESIAN_POINT('Ctrl Pts',(-21.3529920927018,5.9297034129337,0.908025318629945));
#29120=CARTESIAN_POINT('Ctrl Pts',(-21.3994116407294,5.99786700871715,-0.10716291510071));
#29121=CARTESIAN_POINT('Ctrl Pts',(-21.445831188757,5.81850801710345,-1.07655394165592));
#29122=CARTESIAN_POINT('Ctrl Pts',(-21.4922507367846,5.63914902548975,-2.04594496821113));
#29123=CARTESIAN_POINT('Ctrl Pts',(-21.5386702848122,5.2122674464789,-2.9695387875909));
#29124=CARTESIAN_POINT('Ctrl Pts',(-21.5850898328398,4.59011961036565,-3.73427448066272));
#29125=CARTESIAN_POINT('Ctrl Pts',(-21.6315093808674,3.96797177425236,-4.49901017373458));
#29126=CARTESIAN_POINT('Ctrl Pts',(-21.677928928895,3.15055768103664,-5.10488774049848));
#29127=CARTESIAN_POINT('Ctrl Pts',(-21.7243484769227,2.23794035274358,-5.4777392154021));
#29128=CARTESIAN_POINT('Ctrl Pts',(-21.7707680249503,1.32532302445052,-5.85059069030572));
#29129=CARTESIAN_POINT('Ctrl Pts',(-21.8171875729779,0.317502461080135,
-5.99041607334905));
#29130=CARTESIAN_POINT('Ctrl Pts',(-21.8636071210055,-0.662149875990963,
-5.8800987641465));
#29131=CARTESIAN_POINT('Ctrl Pts',(-21.9100266690331,-1.64180221306201,
-5.76978145494396));
#29132=CARTESIAN_POINT('Ctrl Pts',(-21.9564462170607,-2.59328632383376,
-5.40932145349556));
#29133=CARTESIAN_POINT('Ctrl Pts',(-22.0028657650883,-3.40012712386265,
-4.84284415152558));
#29134=CARTESIAN_POINT('Ctrl Pts',(-22.0492853131159,-4.20696792389155,
-4.27636684955561));
#29135=CARTESIAN_POINT('Ctrl Pts',(-22.0957048611436,-4.86916541317758,
-3.50387224706406));
#29136=CARTESIAN_POINT('Ctrl Pts',(-22.1421244091712,-5.30565727275007,
-2.61992458641588));
#29137=CARTESIAN_POINT('Ctrl Pts',(-22.1847078753791,-5.70607772365798,
-1.80902579622443));
#29138=CARTESIAN_POINT('Ctrl Pts',(-22.2272913415871,-5.91655547984308,
-0.904333624679423));
#29139=CARTESIAN_POINT('Ctrl Pts',(-22.2698748077951,-5.91717032569028,
8.22304250084477E-5));
#29140=CARTESIAN_POINT('Ctrl Pts',(-22.5216251922048,-5.91704156442688,
0.000122038191318572));
#29141=CARTESIAN_POINT('Ctrl Pts',(-22.481480804764,-5.91625785823037,-0.852544773504149));
#29142=CARTESIAN_POINT('Ctrl Pts',(-22.4413364173232,-5.7299223214418,-1.70554294837803));
#29143=CARTESIAN_POINT('Ctrl Pts',(-22.4011920298824,-5.37264844600463,
-2.47964765843172));
#29144=CARTESIAN_POINT('Ctrl Pts',(-22.3547724818548,-4.95952738781642,
-3.37475636621097));
#29145=CARTESIAN_POINT('Ctrl Pts',(-22.3083529338272,-4.31785085791257,
-4.16437947485653));
#29146=CARTESIAN_POINT('Ctrl Pts',(-22.2619333857995,-3.52616912020172,
-4.75185597109779));
#29147=CARTESIAN_POINT('Ctrl Pts',(-22.2155138377719,-2.73448738249086,
-5.33933246733905));
#29148=CARTESIAN_POINT('Ctrl Pts',(-22.1690942897443,-1.79280043697301,
-5.72466235117601));
#29149=CARTESIAN_POINT('Ctrl Pts',(-22.1226747417167,-0.816384056787076,
-5.86067580626549));
#29150=CARTESIAN_POINT('Ctrl Pts',(-22.0762551936891,0.160032323398914,
-5.99668926135499));
#29151=CARTESIAN_POINT('Ctrl Pts',(-22.0298356456614,1.17117813825299,-5.88338628769699));
#29152=CARTESIAN_POINT('Ctrl Pts',(-21.9834160976338,2.09327486868419,-5.53463676842998));
#29153=CARTESIAN_POINT('Ctrl Pts',(-21.9369965496062,3.0153715991154,-5.18588724916296));
#29154=CARTESIAN_POINT('Ctrl Pts',(-21.8905770015786,3.84841924512373,-4.60169118428693));
#29155=CARTESIAN_POINT('Ctrl Pts',(-21.844157453551,4.49044101716969,-3.85356241750953));
#29156=CARTESIAN_POINT('Ctrl Pts',(-21.7977379055234,5.13246278921561,-3.10543365073218));
#29157=CARTESIAN_POINT('Ctrl Pts',(-21.7513183574958,5.58345868729917,-2.19337218205349));
#29158=CARTESIAN_POINT('Ctrl Pts',(-21.7048988094682,5.78822044812066,-1.22902720811207));
#29159=CARTESIAN_POINT('Ctrl Pts',(-21.6584792614406,5.99298220894214,-0.264682234170656));
#29160=CARTESIAN_POINT('Ctrl Pts',(-21.612059713413,5.95150983250155,0.751946245033478));
#29161=CARTESIAN_POINT('Ctrl Pts',(-21.5656401653854,5.66888012301801,1.69640855491039));
#29162=CARTESIAN_POINT('Ctrl Pts',(-21.5192206173577,5.38625041353447,2.6408708647873));
#29163=CARTESIAN_POINT('Ctrl Pts',(-21.4728010693301,4.86246337100797,3.51316700533699));
#29164=CARTESIAN_POINT('Ctrl Pts',(-21.4263815213025,4.1616379221952,4.20651561733327));
#29165=CARTESIAN_POINT('Ctrl Pts',(-21.3799619732749,3.46081247338243,4.89986422932954));
#29166=CARTESIAN_POINT('Ctrl Pts',(-21.3335424252473,2.58294861828339,5.41426531277241));
#29167=CARTESIAN_POINT('Ctrl Pts',(-21.2871228772197,1.63550928296806,5.68674891477082));
#29168=CARTESIAN_POINT('Ctrl Pts',(-21.2407033291921,0.68806994765268,5.95923251676925));
#29169=CARTESIAN_POINT('Ctrl Pts',(-21.1942837811644,-0.328944867879004,
5.98979863732319));
#29170=CARTESIAN_POINT('Ctrl Pts',(-21.1478642331368,-1.29103819601777,
5.77470555186539));
#29171=CARTESIAN_POINT('Ctrl Pts',(-21.1014446851092,-2.25313152415654,
5.55961246640759));
#29172=CARTESIAN_POINT('Ctrl Pts',(-21.0550251370816,-3.1603033649024,5.09886017493805));
#29173=CARTESIAN_POINT('Ctrl Pts',(-21.008605589054,-3.90150308108809,4.44885126100907));
#29174=CARTESIAN_POINT('Ctrl Pts',(-20.9621860410264,-4.6427027972737,3.79884234708015));
#29175=CARTESIAN_POINT('Ctrl Pts',(-20.9157664929988,-5.21793038889919,
2.95957681069184));
#29176=CARTESIAN_POINT('Ctrl Pts',(-20.8693469449712,-5.55676987996417,
2.03379259892567));
#29177=CARTESIAN_POINT('Ctrl Pts',(-20.8367730273824,-5.79454319157011,
1.38414347694089));
#29178=CARTESIAN_POINT('Ctrl Pts',(-20.8041991097936,-5.91591360793864,
0.691890584790816));
#29179=CARTESIAN_POINT('Ctrl Pts',(-20.7716251922048,-5.9165474513811,-0.000145824772724381));
#29180=CARTESIAN_POINT('Origin',(-29.75,0.,0.));
#29181=CARTESIAN_POINT('',(-18.7698748077951,-5.91679704493989,0.000153720370225236));
#29182=CARTESIAN_POINT('',(-19.0216251922048,-5.91663428088003,0.000153302805156978));
#29183=CARTESIAN_POINT('',(-29.75,-5.91675,-7.2459289488551E-16));
#29184=CARTESIAN_POINT('Ctrl Pts',(-18.7698748077951,-5.91679704493989,
0.000153720370225235));
#29185=CARTESIAN_POINT('Ctrl Pts',(-18.7798888555911,-5.91701835347429,
0.212877460640914));
#29186=CARTESIAN_POINT('Ctrl Pts',(-18.7899029033871,-5.90576990250038,
0.425577918591127));
#29187=CARTESIAN_POINT('Ctrl Pts',(-18.7999169511831,-5.88287455300957,
0.637017211654891));
#29188=CARTESIAN_POINT('Ctrl Pts',(-18.8463364992107,-5.77674446486252,
1.61713200831315));
#29189=CARTESIAN_POINT('Ctrl Pts',(-18.8927560472383,-5.42035360085787,
2.57014773627856));
#29190=CARTESIAN_POINT('Ctrl Pts',(-18.9391755952659,-4.85732923286482,
3.37940181954573));
#29191=CARTESIAN_POINT('Ctrl Pts',(-18.9855951432935,-4.29430486487177,
4.1886559028129));
#29192=CARTESIAN_POINT('Ctrl Pts',(-19.0320146913211,-3.52464699289032,
4.85414834138182));
#29193=CARTESIAN_POINT('Ctrl Pts',(-19.0784342393488,-2.64257260343326,
5.29441346798454));
#29194=CARTESIAN_POINT('Ctrl Pts',(-19.1248537873764,-1.76049821397624,
5.73467859458724));
#29195=CARTESIAN_POINT('Ctrl Pts',(-19.171273335404,-0.766007307043637,
5.94971640922375));
#29196=CARTESIAN_POINT('Ctrl Pts',(-19.2176928834316,0.219160394071264,
5.91320324833018));
#29197=CARTESIAN_POINT('Ctrl Pts',(-19.2641124314592,1.20432809518617,5.87669008743662));
#29198=CARTESIAN_POINT('Ctrl Pts',(-19.3105319794868,2.18017259048333,5.58862595101298));
#29199=CARTESIAN_POINT('Ctrl Pts',(-19.3569515275144,3.02723674062986,5.08427395510635));
#29200=CARTESIAN_POINT('Ctrl Pts',(-19.403371075542,3.87430089077639,4.57992195919972));
#29201=CARTESIAN_POINT('Ctrl Pts',(-19.4497906235696,4.59258469577225,3.85928210381012));
#29202=CARTESIAN_POINT('Ctrl Pts',(-19.4962101715973,5.09416007999938,3.01057087837719));
#29203=CARTESIAN_POINT('Ctrl Pts',(-19.5426297196249,5.59573546422651,2.16185965294427));
#29204=CARTESIAN_POINT('Ctrl Pts',(-19.5890492676525,5.88060242768489,1.18507705746804));
#29205=CARTESIAN_POINT('Ctrl Pts',(-19.6354688156801,5.91388923342342,0.199795067983714));
#29206=CARTESIAN_POINT('Ctrl Pts',(-19.6818883637077,5.94717603916195,-0.785486921500666));
#29207=CARTESIAN_POINT('Ctrl Pts',(-19.7283079117353,5.72888268718055,-1.77926830499326));
#29208=CARTESIAN_POINT('Ctrl Pts',(-19.7747274597629,5.28573136476298,-2.65989621488377));
#29209=CARTESIAN_POINT('Ctrl Pts',(-19.8211470077906,4.84258004234542,-3.54052412477423));
#29210=CARTESIAN_POINT('Ctrl Pts',(-19.8675665558182,4.17457074949172,-4.30799856106274));
#29211=CARTESIAN_POINT('Ctrl Pts',(-19.9139861038458,3.36347725195724,-4.86836982058248));
#29212=CARTESIAN_POINT('Ctrl Pts',(-19.9604056518734,2.55238375442275,-5.42874108010222));
#29213=CARTESIAN_POINT('Ctrl Pts',(-20.006825199901,1.59820605220752,-5.78200916285315));
#29214=CARTESIAN_POINT('Ctrl Pts',(-20.0532447479286,0.617748963365208,
-5.88492906946662));
#29215=CARTESIAN_POINT('Ctrl Pts',(-20.0996642959562,-0.362708125477101,
-5.98784897608009));
#29216=CARTESIAN_POINT('Ctrl Pts',(-20.1460838439838,-1.36944460094645,
-5.84042070655609));
#29217=CARTESIAN_POINT('Ctrl Pts',(-20.1925033920114,-2.27922170932619,
-5.4606915618929));
#29218=CARTESIAN_POINT('Ctrl Pts',(-20.2389229400391,-3.18899881770599,
-5.08096241722968));
#29219=CARTESIAN_POINT('Ctrl Pts',(-20.2853424880667,-4.00181655899615,
-4.46893239742725));
#29220=CARTESIAN_POINT('Ctrl Pts',(-20.3317620360943,-4.61817456952039,
-3.6995226151258));
#29221=CARTESIAN_POINT('Ctrl Pts',(-20.3781815841219,-5.23453258004463,
-2.93011283282435));
#29222=CARTESIAN_POINT('Ctrl Pts',(-20.4246011321495,-5.65443085980294,
-2.0033232880239));
#29223=CARTESIAN_POINT('Ctrl Pts',(-20.4710206801771,-5.82646793289164,
-1.03260610175302));
#29224=CARTESIAN_POINT('Ctrl Pts',(-20.4873053893831,-5.8868212501241,-0.692063210420498));
#29225=CARTESIAN_POINT('Ctrl Pts',(-20.5035900985891,-5.91666986722,-0.346114069563229));
#29226=CARTESIAN_POINT('Ctrl Pts',(-20.5198748077951,-5.91641453668928,
-0.000121371007781868));
#29227=CARTESIAN_POINT('Ctrl Pts',(-20.7716251922048,-5.9165474513811,-0.000145824772724381));
#29228=CARTESIAN_POINT('Ctrl Pts',(-20.757779561766,-5.9168168682247,-0.294297744047323));
#29229=CARTESIAN_POINT('Ctrl Pts',(-20.7439339313272,-5.8952728365774,-0.588410551463468));
#29230=CARTESIAN_POINT('Ctrl Pts',(-20.7300883008883,-5.85158255527674,
-0.87919590143652));
#29231=CARTESIAN_POINT('Ctrl Pts',(-20.6836687528607,-5.70510434901984,
-1.8540973028883));
#29232=CARTESIAN_POINT('Ctrl Pts',(-20.6372492048331,-5.30969654600157,
-2.79159721864773));
#29233=CARTESIAN_POINT('Ctrl Pts',(-20.5908296568055,-4.71376264211306,
-3.57693242711421));
#29234=CARTESIAN_POINT('Ctrl Pts',(-20.5444101087779,-4.11782873822455,
-4.3622676355807));
#29235=CARTESIAN_POINT('Ctrl Pts',(-20.4979905607502,-3.32136873346579,
-4.99543813675423));
#29236=CARTESIAN_POINT('Ctrl Pts',(-20.4515710127226,-2.4218805736879,-5.39893492469718));
#29237=CARTESIAN_POINT('Ctrl Pts',(-20.405151464695,-1.52239241391001,-5.80243171264014));
#29238=CARTESIAN_POINT('Ctrl Pts',(-20.3587319166674,-0.519876099112993,
-5.97625478735251));
#29239=CARTESIAN_POINT('Ctrl Pts',(-20.3123123686398,0.462946224216296,
-5.89912575114362));
#29240=CARTESIAN_POINT('Ctrl Pts',(-20.2658928206122,1.44576854754547,-5.82199671493473));
#29241=CARTESIAN_POINT('Ctrl Pts',(-20.2194732725846,2.40889687940692,-5.49391556780463));
#29242=CARTESIAN_POINT('Ctrl Pts',(-20.173053724557,3.2344307183487,-4.95504407271259));
#29243=CARTESIAN_POINT('Ctrl Pts',(-20.1266341765294,4.05996455729051,-4.41617257762052));
#29244=CARTESIAN_POINT('Ctrl Pts',(-20.0802146285017,4.74790390331264,-3.66651073456648));
#29245=CARTESIAN_POINT('Ctrl Pts',(-20.0337950804741,5.21403527085829,-2.79782773389776));
#29246=CARTESIAN_POINT('Ctrl Pts',(-19.9873755324465,5.68016663840395,-1.92914473322905));
#29247=CARTESIAN_POINT('Ctrl Pts',(-19.9409559844189,5.92449002747313,-0.941440574945666));
#29248=CARTESIAN_POINT('Ctrl Pts',(-19.8945364363913,5.91709680685361,0.0443758114821791));
#29249=CARTESIAN_POINT('Ctrl Pts',(-19.8481168883637,5.90970358623408,1.03019219791008));
#29250=CARTESIAN_POINT('Ctrl Pts',(-19.8016973403361,5.65059375592582,2.01412081248244));
#29251=CARTESIAN_POINT('Ctrl Pts',(-19.7552777923085,5.17148601624514,2.87571490556745));
#29252=CARTESIAN_POINT('Ctrl Pts',(-19.7088582442808,4.69237827656447,3.73730899865245));
#29253=CARTESIAN_POINT('Ctrl Pts',(-19.6624386962532,3.99327262751139,4.47656857025009));
#29254=CARTESIAN_POINT('Ctrl Pts',(-19.6160191482256,3.15974946773534,5.00299781485742));
#29255=CARTESIAN_POINT('Ctrl Pts',(-19.569599600198,2.32622630795928,5.52942705946474));
#29256=CARTESIAN_POINT('Ctrl Pts',(-19.5231800521704,1.35828563746025,5.84302597708174));
#29257=CARTESIAN_POINT('Ctrl Pts',(-19.4767605041428,0.374417055861,5.90540563404431));
#29258=CARTESIAN_POINT('Ctrl Pts',(-19.4303409561152,-0.609451525738141,
5.96778529100687));
#29259=CARTESIAN_POINT('Ctrl Pts',(-19.3839214080876,-1.6092480184375,5.77894568731507));
#29260=CARTESIAN_POINT('Ctrl Pts',(-19.33750186006,-2.50258322036267,5.36200345575057));
#29261=CARTESIAN_POINT('Ctrl Pts',(-19.2910823120323,-3.39591842228794,
4.94506122418602));
#29262=CARTESIAN_POINT('Ctrl Pts',(-19.2446627640047,-4.182792333439,4.30001636474871));
#29263=CARTESIAN_POINT('Ctrl Pts',(-19.1982432159771,-4.76688048112083,
3.50583147242293));
#29264=CARTESIAN_POINT('Ctrl Pts',(-19.1518236679495,-5.35096862880262,
2.7116465800972));
#29265=CARTESIAN_POINT('Ctrl Pts',(-19.1054041199219,-5.73227101301522,
1.76832165488302));
#29266=CARTESIAN_POINT('Ctrl Pts',(-19.0589845718943,-5.86411084021375,
0.791332981752648));
#29267=CARTESIAN_POINT('Ctrl Pts',(-19.0465314453311,-5.89947994921908,
0.529232980476941));
#29268=CARTESIAN_POINT('Ctrl Pts',(-19.034078318768,-5.91689509388119,0.264710179816106));
#29269=CARTESIAN_POINT('Ctrl Pts',(-19.0216251922048,-5.91663428088003,
0.000153302805156978));
#29270=CARTESIAN_POINT('Origin',(-29.75,0.,0.));
#29271=CARTESIAN_POINT('',(-17.0198748077951,-5.916790746513,-0.000154010032091534));
#29272=CARTESIAN_POINT('',(-17.2716251922048,-5.91695431715726,-0.000138309308396116));
#29273=CARTESIAN_POINT('',(-29.75,-5.91675,-7.2459289488551E-16));
#29274=CARTESIAN_POINT('Ctrl Pts',(-17.0198748077951,-5.916790746513,-0.000154010032091534));
#29275=CARTESIAN_POINT('Ctrl Pts',(-17.0561876125931,-5.91598848246282,
0.771224306268274));
#29276=CARTESIAN_POINT('Ctrl Pts',(-17.0925004173911,-5.76438952161292,
1.54290865794934));
#29277=CARTESIAN_POINT('Ctrl Pts',(-17.128813222189,-5.47038119103934,2.25586647634896));
#29278=CARTESIAN_POINT('Ctrl Pts',(-17.1752327702167,-5.09454313893885,
3.1672579228919));
#29279=CARTESIAN_POINT('Ctrl Pts',(-17.2216523182443,-4.48599200945246,
3.98268354702695));
#29280=CARTESIAN_POINT('Ctrl Pts',(-17.2680718662719,-3.71922304994449,
4.60232374340981));
#29281=CARTESIAN_POINT('Ctrl Pts',(-17.3144914142995,-2.95245409043648,
5.22196393979271));
#29282=CARTESIAN_POINT('Ctrl Pts',(-17.3609109623271,-2.02746730090685,
5.64581870842343));
#29283=CARTESIAN_POINT('Ctrl Pts',(-17.4073305103547,-1.05749411969492,
5.82200224331825));
#29284=CARTESIAN_POINT('Ctrl Pts',(-17.4537500583823,-0.087520938482929,
5.99818577821308));
#29285=CARTESIAN_POINT('Ctrl Pts',(-17.5001696064099,0.927438634411407,
5.926698079372));
#29286=CARTESIAN_POINT('Ctrl Pts',(-17.5465891544375,1.86313922208543,5.61629025011341));
#29287=CARTESIAN_POINT('Ctrl Pts',(-17.5930087024651,2.79883980975946,5.30588242085483));
#29288=CARTESIAN_POINT('Ctrl Pts',(-17.6394282504928,3.65528141221321,4.75655446117873));
#29289=CARTESIAN_POINT('Ctrl Pts',(-17.6858477985204,4.32762348945498,4.03555186658647));
#29290=CARTESIAN_POINT('Ctrl Pts',(-17.732267346548,4.99996556669675,3.31454927199422));
#29291=CARTESIAN_POINT('Ctrl Pts',(-17.7786868945756,5.48820811872651,2.42187204248595));
#29292=CARTESIAN_POINT('Ctrl Pts',(-17.8251064426032,5.73258336610087,1.46679647023563));
#29293=CARTESIAN_POINT('Ctrl Pts',(-17.8715259906308,5.97695861347522,0.511720897985363));
#29294=CARTESIAN_POINT('Ctrl Pts',(-17.9179455386584,5.97746655619411,-0.505753017006816));
#29295=CARTESIAN_POINT('Ctrl Pts',(-17.964365086686,5.73404501489963,-1.46107210687797));
#29296=CARTESIAN_POINT('Ctrl Pts',(-18.0107846347137,5.49062347360513,-2.41639119674918));
#29297=CARTESIAN_POINT('Ctrl Pts',(-18.0572041827413,5.00327244829723,-3.30955546149939));
#29298=CARTESIAN_POINT('Ctrl Pts',(-18.1036237307689,4.33165058296566,-4.03122898896668));
#29299=CARTESIAN_POINT('Ctrl Pts',(-18.1500432787965,3.66002871763409,-4.75290251643397));
#29300=CARTESIAN_POINT('Ctrl Pts',(-18.1964628268241,2.80413601227882,-5.30308530661837));
#29301=CARTESIAN_POINT('Ctrl Pts',(-18.2428823748517,1.86874581413954,-5.61442722069919));
#29302=CARTESIAN_POINT('Ctrl Pts',(-18.2893019228793,0.933355616000316,
-5.92576913477999));
#29303=CARTESIAN_POINT('Ctrl Pts',(-18.335721470907,-0.0815320749229426,
-5.99827017275724));
#29304=CARTESIAN_POINT('Ctrl Pts',(-18.3821410189346,-1.05168068109539,
-5.82305518429997));
#29305=CARTESIAN_POINT('Ctrl Pts',(-18.4285605669622,-2.02182928726785,
-5.6478401958427));
#29306=CARTESIAN_POINT('Ctrl Pts',(-18.4749801149898,-2.94723880868953,
-5.22490918095089));
#29307=CARTESIAN_POINT('Ctrl Pts',(-18.5213996630174,-3.71462605867108,
-4.60603486511271));
#29308=CARTESIAN_POINT('Ctrl Pts',(-18.567819211045,-4.48201330865264,-3.98716054927452));
#29309=CARTESIAN_POINT('Ctrl Pts',(-18.6142387590726,-5.0913782871941,-3.17234293248995));
#29310=CARTESIAN_POINT('Ctrl Pts',(-18.6606583071002,-5.46812612032009,
-2.26132719142216));
#29311=CARTESIAN_POINT('Ctrl Pts',(-18.6970638073319,-5.76359847860266,
-1.54684406563382));
#29312=CARTESIAN_POINT('Ctrl Pts',(-18.7334693075635,-5.9159924903717,-0.773191317866126));
#29313=CARTESIAN_POINT('Ctrl Pts',(-18.7698748077951,-5.91679704493989,
0.000153720370225235));
#29314=CARTESIAN_POINT('Ctrl Pts',(-19.0216251922048,-5.91663428088003,
0.000153302805156978));
#29315=CARTESIAN_POINT('Ctrl Pts',(-18.9876587707404,-5.91592290255459,
-0.721436599964167));
#29316=CARTESIAN_POINT('Ctrl Pts',(-18.9536923492759,-5.78371152898367,
-1.44328001317763));
#29317=CARTESIAN_POINT('Ctrl Pts',(-18.9197259278114,-5.52564133302854,
-2.11690616066192));
#29318=CARTESIAN_POINT('Ctrl Pts',(-18.8733063797838,-5.17295472846031,
-3.0375042088996));
#29319=CARTESIAN_POINT('Ctrl Pts',(-18.8268868317562,-4.58520424913938,
-3.86804788432833));
#29320=CARTESIAN_POINT('Ctrl Pts',(-18.7804672837286,-3.83433884926859,
-4.50686691874871));
#29321=CARTESIAN_POINT('Ctrl Pts',(-18.734047735701,-3.08347344939785,-5.14568595316904));
#29322=CARTESIAN_POINT('Ctrl Pts',(-18.6876281876734,-2.16949312897728,
-5.59278034658103));
#29323=CARTESIAN_POINT('Ctrl Pts',(-18.6412086396458,-1.20428197918144,
-5.79341943492276));
#29324=CARTESIAN_POINT('Ctrl Pts',(-18.5947890916182,-0.239070829385605,
-5.99405852326448));
#29325=CARTESIAN_POINT('Ctrl Pts',(-18.5483695435905,0.777371149785462,
-5.94824230653593));
#29326=CARTESIAN_POINT('Ctrl Pts',(-18.5019499955629,1.72061711397817,-5.66157933631661));
#29327=CARTESIAN_POINT('Ctrl Pts',(-18.4555304475353,2.66386307817093,-5.37491636609728));
#29328=CARTESIAN_POINT('Ctrl Pts',(-18.4091108995077,3.5339130273853,-4.84740664238717));
#29329=CARTESIAN_POINT('Ctrl Pts',(-18.3626913514801,4.22426056791737,-4.14362480066189));
#29330=CARTESIAN_POINT('Ctrl Pts',(-18.3162718034525,4.9146081084494,-3.43984295893665));
#29331=CARTESIAN_POINT('Ctrl Pts',(-18.2698522554248,5.42525324029921,-2.55978899919613));
#29332=CARTESIAN_POINT('Ctrl Pts',(-18.2234327073972,5.69368579206225,-1.61119394722993));
#29333=CARTESIAN_POINT('Ctrl Pts',(-18.1770131593696,5.9621183438253,-0.662598895263667));
#29334=CARTESIAN_POINT('Ctrl Pts',(-18.130593611342,5.98833831550164,0.354537248928418));
#29335=CARTESIAN_POINT('Ctrl Pts',(-18.0841740633144,5.76913601248835,1.31570266539666));
#29336=CARTESIAN_POINT('Ctrl Pts',(-18.0377545152868,5.54993370947507,2.27686808186486));
#29337=CARTESIAN_POINT('Ctrl Pts',(-17.9913349672592,5.08530913177228,3.18206277060904));
#29338=CARTESIAN_POINT('Ctrl Pts',(-17.9449154192316,4.43213888542068,3.9204781257729));
#29339=CARTESIAN_POINT('Ctrl Pts',(-17.898495871204,3.77896863906908,4.65889348093676));
#29340=CARTESIAN_POINT('Ctrl Pts',(-17.8520763231763,2.93725272406858,5.23052950252021));
#29341=CARTESIAN_POINT('Ctrl Pts',(-17.8056567751487,2.01002904842788,5.5654098733874));
#29342=CARTESIAN_POINT('Ctrl Pts',(-17.7592372271211,1.08280537278718,5.90029024425459));
#29343=CARTESIAN_POINT('Ctrl Pts',(-17.7128176790935,0.0700739365061698,
5.99841496440561));
#29344=CARTESIAN_POINT('Ctrl Pts',(-17.6663981310659,-0.904192638882054,
5.84777218315773));
#29345=CARTESIAN_POINT('Ctrl Pts',(-17.6199785830383,-1.87845921427028,
5.69712940190986));
#29346=CARTESIAN_POINT('Ctrl Pts',(-17.5735590350107,-2.81426092876568,
5.29771911926308));
#29347=CARTESIAN_POINT('Ctrl Pts',(-17.5271394869831,-3.59704244457092,
4.69843479110619));
#29348=CARTESIAN_POINT('Ctrl Pts',(-17.4807199389554,-4.3798239603762,4.09915046294928));
#29349=CARTESIAN_POINT('Ctrl Pts',(-17.4343003909278,-5.00958527749128,
3.29999208928225));
#29350=CARTESIAN_POINT('Ctrl Pts',(-17.3878808429002,-5.40923472222464,
2.39878793439545));
#29351=CARTESIAN_POINT('Ctrl Pts',(-17.3491289593351,-5.74286935261707,
1.64644630328328));
#29352=CARTESIAN_POINT('Ctrl Pts',(-17.31037707577,-5.91613408823061,0.822986780567107));
#29353=CARTESIAN_POINT('Ctrl Pts',(-17.2716251922048,-5.91695431715726,
-0.000138309308396116));
#29354=CARTESIAN_POINT('Origin',(-29.75,0.,0.));
#29355=CARTESIAN_POINT('',(-15.2698748077951,-5.91641904191932,0.000122539150512468));
#29356=CARTESIAN_POINT('',(-15.5216251922048,-5.91631764548591,8.65724823460925E-5));
#29357=CARTESIAN_POINT('',(-29.75,-5.91675,-7.2459289488551E-16));
#29358=CARTESIAN_POINT('Ctrl Pts',(-15.2698748077951,-5.91641904191932,
0.000122539150512468));
#29359=CARTESIAN_POINT('Ctrl Pts',(-15.2860668215674,-5.91667562844659,
0.344145035781405));
#29360=CARTESIAN_POINT('Ctrl Pts',(-15.3022588353398,-5.88716769234933,
0.688124008340338));
#29361=CARTESIAN_POINT('Ctrl Pts',(-15.3184508491121,-5.82749602249077,
1.02678821684237));
#29362=CARTESIAN_POINT('Ctrl Pts',(-15.3648703971398,-5.65642823661614,
1.99767668771552));
#29363=CARTESIAN_POINT('Ctrl Pts',(-15.4112899451674,-5.23745550856503,
2.92488501319836));
#29364=CARTESIAN_POINT('Ctrl Pts',(-15.457709493195,-4.62186601364884,3.6949098075961));
#29365=CARTESIAN_POINT('Ctrl Pts',(-15.5041290412226,-4.00627651873265,
4.46493460199384));
#29366=CARTESIAN_POINT('Ctrl Pts',(-15.5505485892502,-3.1940702569514,5.07777586530647));
#29367=CARTESIAN_POINT('Ctrl Pts',(-15.5969681372778,-2.28467273825905,
5.45841317723823));
#29368=CARTESIAN_POINT('Ctrl Pts',(-15.6433876853054,-1.37527521956669,
5.83905048916999));
#29369=CARTESIAN_POINT('Ctrl Pts',(-15.689807233333,-0.368686443963233,
5.98748384972087));
#29370=CARTESIAN_POINT('Ctrl Pts',(-15.7362267813607,0.611872915382893,
5.88554292056501));
#29371=CARTESIAN_POINT('Ctrl Pts',(-15.7826463293883,1.59243227472908,5.78360199140914));
#29372=CARTESIAN_POINT('Ctrl Pts',(-15.8290658774159,2.54696221781793,5.43128677254651));
#29373=CARTESIAN_POINT('Ctrl Pts',(-15.8754854254435,3.35861480734123,4.8717256193571));
#29374=CARTESIAN_POINT('Ctrl Pts',(-15.9219049734711,4.1702673968645,4.31216446616772));
#29375=CARTESIAN_POINT('Ctrl Pts',(-15.9683245214987,4.83904263282224,3.5453573786516));
#29376=CARTESIAN_POINT('Ctrl Pts',(-16.0147440695263,5.28307298721258,2.66517236706686));
#29377=CARTESIAN_POINT('Ctrl Pts',(-16.0611636175539,5.72710334160293,1.78498735548211));
#29378=CARTESIAN_POINT('Ctrl Pts',(-16.1075831655815,5.94638881442588,0.791424419828757));
#29379=CARTESIAN_POINT('Ctrl Pts',(-16.1540027136092,5.9140857688039,-0.193890313381902));
#29380=CARTESIAN_POINT('Ctrl Pts',(-16.2004222616368,5.88178272318191,-1.17920504659262));
#29381=CARTESIAN_POINT('Ctrl Pts',(-16.2468418096644,5.59789115911495,-2.15627157736063));
#29382=CARTESIAN_POINT('Ctrl Pts',(-16.293261357692,5.09716341090182,-3.00548317196351));
#29383=CARTESIAN_POINT('Ctrl Pts',(-16.3396809057196,4.59643566268871,-3.85469476656634));
#29384=CARTESIAN_POINT('Ctrl Pts',(-16.3861004537472,3.87887173032945,-4.57605142500404));
#29385=CARTESIAN_POINT('Ctrl Pts',(-16.4325200017748,3.03231156687109,-5.08124891102688));
#29386=CARTESIAN_POINT('Ctrl Pts',(-16.4789395498025,2.18575140341273,-5.58644639704972));
#29387=CARTESIAN_POINT('Ctrl Pts',(-16.5253590978301,1.21019500885526,-5.87548471065769));
#29388=CARTESIAN_POINT('Ctrl Pts',(-16.5717786458577,0.225064254934827,
-5.91298148276677));
#29389=CARTESIAN_POINT('Ctrl Pts',(-16.6181981938853,-0.760066498985666,
-5.95047825487585));
#29390=CARTESIAN_POINT('Ctrl Pts',(-16.6646177419129,-1.75477161226913,
-5.736433485486));
#29391=CARTESIAN_POINT('Ctrl Pts',(-16.7110372899405,-2.63728513974157,
-5.29704927540705));
#29392=CARTESIAN_POINT('Ctrl Pts',(-16.7574568379681,-3.51979866721402,
-4.8576650653281));
#29393=CARTESIAN_POINT('Ctrl Pts',(-16.8038763859957,-4.29012060887544,
-4.19294141456005));
#29394=CARTESIAN_POINT('Ctrl Pts',(-16.8502959340234,-4.85395268671152,
-3.38424987989334));
#29395=CARTESIAN_POINT('Ctrl Pts',(-16.896715482051,-5.4177847645476,-2.57555834522663));
#29396=CARTESIAN_POINT('Ctrl Pts',(-16.9431350300786,-5.77512697855834,
-1.62289892666125));
#29397=CARTESIAN_POINT('Ctrl Pts',(-16.9895545781062,-5.8822355982064,-0.642890582903073));
#29398=CARTESIAN_POINT('Ctrl Pts',(-16.9996613213358,-5.90555593117947,
-0.429517271138596));
#29399=CARTESIAN_POINT('Ctrl Pts',(-17.0097680645655,-5.91701403625343,
-0.214847494028373));
#29400=CARTESIAN_POINT('Ctrl Pts',(-17.0198748077951,-5.916790746513,-0.000154010032091534));
#29401=CARTESIAN_POINT('Ctrl Pts',(-17.2716251922048,-5.91695431715726,
-0.000138309308396116));
#29402=CARTESIAN_POINT('Ctrl Pts',(-17.2639575277424,-5.9171166122411,-0.163006444200649));
#29403=CARTESIAN_POINT('Ctrl Pts',(-17.2562898632799,-5.91052756808586,
-0.325861485781881));
#29404=CARTESIAN_POINT('Ctrl Pts',(-17.2486221988174,-5.89709364756359,
-0.488149921834486));
#29405=CARTESIAN_POINT('Ctrl Pts',(-17.2022026507898,-5.81576555581756,
-1.47063368707121));
#29406=CARTESIAN_POINT('Ctrl Pts',(-17.1557831027622,-5.48357179997386,
-2.43235128143819));
#29407=CARTESIAN_POINT('Ctrl Pts',(-17.1093635547345,-4.94117758434384,
-3.25557489766398));
#29408=CARTESIAN_POINT('Ctrl Pts',(-17.0629440067069,-4.39878336871378,
-4.07879851388981));
#29409=CARTESIAN_POINT('Ctrl Pts',(-17.0165244586793,-3.64618869329736,
-4.76352815197446));
#29410=CARTESIAN_POINT('Ctrl Pts',(-16.9701049106517,-2.77552176851717,
-5.2259432399146));
#29411=CARTESIAN_POINT('Ctrl Pts',(-16.9236853626241,-1.90485484373698,
-5.68835832785475));
#29412=CARTESIAN_POINT('Ctrl Pts',(-16.8772658145965,-0.916115669593002,
-5.92845886565041));
#29413=CARTESIAN_POINT('Ctrl Pts',(-16.8308462665689,0.0696601238949256,
-5.9168531586867));
#29414=CARTESIAN_POINT('Ctrl Pts',(-16.7844267185412,1.05543591738285,-5.905247451723));
#29415=CARTESIAN_POINT('Ctrl Pts',(-16.7380071705136,2.03824833021476,-5.64193549999993));
#29416=CARTESIAN_POINT('Ctrl Pts',(-16.691587622486,2.89778725160595,-5.15915040280392));
#29417=CARTESIAN_POINT('Ctrl Pts',(-16.6451680744584,3.75732617299704,-4.67636530560797));
#29418=CARTESIAN_POINT('Ctrl Pts',(-16.5987485264308,4.49359160294746,-3.97410706293911));
#29419=CARTESIAN_POINT('Ctrl Pts',(-16.5523289784032,5.01645426115131,-3.13834199540119));
#29420=CARTESIAN_POINT('Ctrl Pts',(-16.5059094303756,5.53931691935521,-2.30257692786317));
#29421=CARTESIAN_POINT('Ctrl Pts',(-16.459489882348,5.84877680581247,-1.3333050354562));
#29422=CARTESIAN_POINT('Ctrl Pts',(-16.4130703343204,5.90695166269147,-0.349178878153185));
#29423=CARTESIAN_POINT('Ctrl Pts',(-16.3666507862928,5.96512651957047,0.634947279149776));
#29424=CARTESIAN_POINT('Ctrl Pts',(-16.3202312382651,5.77201634687118,1.63392770134863));
#29425=CARTESIAN_POINT('Ctrl Pts',(-16.2738116902375,5.35126055529678,2.52547308511626));
#29426=CARTESIAN_POINT('Ctrl Pts',(-16.2273921422099,4.93050476372235,3.41701846888394));
#29427=CARTESIAN_POINT('Ctrl Pts',(-16.1809725941823,4.28210335327276,4.2011288142204));
#29428=CARTESIAN_POINT('Ctrl Pts',(-16.1345530461547,3.48542980815072,4.78181794789139));
#29429=CARTESIAN_POINT('Ctrl Pts',(-16.0881334981271,2.68875626302869,5.36250708156239));
#29430=CARTESIAN_POINT('Ctrl Pts',(-16.0417139500994,1.74381058323418,5.73977500356793));
#29431=CARTESIAN_POINT('Ctrl Pts',(-15.9952944020718,0.76626745697552,5.86743879547986));
#29432=CARTESIAN_POINT('Ctrl Pts',(-15.9488748540442,-0.211275669283083,
5.99510258739178));
#29433=CARTESIAN_POINT('Ctrl Pts',(-15.9024553060166,-1.22141624200586,
5.87316224921013));
#29434=CARTESIAN_POINT('Ctrl Pts',(-15.856035757989,-2.14049879792674,5.51654499939918));
#29435=CARTESIAN_POINT('Ctrl Pts',(-15.8096162099614,-3.05958135384761,
5.15992774958823));
#29436=CARTESIAN_POINT('Ctrl Pts',(-15.7631966619338,-3.88760589296661,
4.56863358814798));
#29437=CARTESIAN_POINT('Ctrl Pts',(-15.7167771139062,-4.52321052492381,
3.81504526598837));
#29438=CARTESIAN_POINT('Ctrl Pts',(-15.6703575658785,-5.15881515688104,
3.06145694382872));
#29439=CARTESIAN_POINT('Ctrl Pts',(-15.6239380178509,-5.60199988167648,
2.14557446094968));
#29440=CARTESIAN_POINT('Ctrl Pts',(-15.5775184698233,-5.79851263386804,
1.17951476005797));
#29441=CARTESIAN_POINT('Ctrl Pts',(-15.5588873772838,-5.87738559637715,
0.791774067811633));
#29442=CARTESIAN_POINT('Ctrl Pts',(-15.5402562847443,-5.91652159902753,
0.395950211203544));
#29443=CARTESIAN_POINT('Ctrl Pts',(-15.5216251922048,-5.91631764548591,
8.65724823460925E-5));
#29444=CARTESIAN_POINT('Origin',(-29.75,0.,0.));
#29445=CARTESIAN_POINT('',(-13.5198748077951,-5.91716619296352,-8.39733533108955E-5));
#29446=CARTESIAN_POINT('',(-13.7716251922048,-5.91724766713751,-3.36308197105027E-5));
#29447=CARTESIAN_POINT('',(-29.75,-5.91675,-7.2459289488551E-16));
#29448=CARTESIAN_POINT('Ctrl Pts',(-13.5198748077951,-5.91716619296352,
-8.39733533108955E-5));
#29449=CARTESIAN_POINT('Ctrl Pts',(-13.5623655785694,-5.91654215140973,
0.9023649832068));
#29450=CARTESIAN_POINT('Ctrl Pts',(-13.6048563493438,-5.7070112106254,1.8050937555527));
#29451=CARTESIAN_POINT('Ctrl Pts',(-13.6473471201181,-5.30827046191485,
2.61462590776469));
#29452=CARTESIAN_POINT('Ctrl Pts',(-13.6937666681457,-4.87266138733159,
3.49900893811922));
#29453=CARTESIAN_POINT('Ctrl Pts',(-13.7401862161733,-4.21123551650526,
4.27216431907237));
#29454=CARTESIAN_POINT('Ctrl Pts',(-13.7866057642009,-3.40496071141642,
4.83944691964926));
#29455=CARTESIAN_POINT('Ctrl Pts',(-13.8330253122285,-2.59868590632748,
5.40672952022621));
#29456=CARTESIAN_POINT('Ctrl Pts',(-13.8794448602561,-1.64756216697599,
5.76813934042686));
#29457=CARTESIAN_POINT('Ctrl Pts',(-13.9258644082838,-0.668020463257402,
5.87943471730586));
#29458=CARTESIAN_POINT('Ctrl Pts',(-13.9722839563114,0.311521240461189,
5.99073009418486));
#29459=CARTESIAN_POINT('Ctrl Pts',(-14.018703504339,1.31948090854688,5.85191102774222));
#29460=CARTESIAN_POINT('Ctrl Pts',(-14.0651230523666,2.23247005124256,5.4799709310084));
#29461=CARTESIAN_POINT('Ctrl Pts',(-14.1115426003942,3.1454591939382,5.10803083427462));
#29462=CARTESIAN_POINT('Ctrl Pts',(-14.1579621484218,3.96347781124383,4.50296970724969));
#29463=CARTESIAN_POINT('Ctrl Pts',(-14.2043816964494,4.58638887885351,3.73885557173862));
#29464=CARTESIAN_POINT('Ctrl Pts',(-14.250801244477,5.20929994646318,2.97474143622756));
#29465=CARTESIAN_POINT('Ctrl Pts',(-14.2972207925047,5.6371034643769,2.05157429223036));
#29466=CARTESIAN_POINT('Ctrl Pts',(-14.3436403405323,5.81743024396591,1.08236282779058));
#29467=CARTESIAN_POINT('Ctrl Pts',(-14.3900598885599,5.99775702355493,0.113151363350743));
#29468=CARTESIAN_POINT('Ctrl Pts',(-14.4364794365875,5.93060706481922,-0.902104421531676));
#29469=CARTESIAN_POINT('Ctrl Pts',(-14.4828989846151,5.62420047046525,-1.83912288942596));
#29470=CARTESIAN_POINT('Ctrl Pts',(-14.5293185326427,5.31779387611128,-2.77614135732025));
#29471=CARTESIAN_POINT('Ctrl Pts',(-14.5757380806703,4.77213064613906,-3.63492250822641));
#29472=CARTESIAN_POINT('Ctrl Pts',(-14.6221576286979,4.05400766141003,-4.31033940840172));
#29473=CARTESIAN_POINT('Ctrl Pts',(-14.6685771767256,3.33588467668099,-4.98575630857702));
#29474=CARTESIAN_POINT('Ctrl Pts',(-14.7149967247532,2.44530193719514,-5.47780895802147));
#29475=CARTESIAN_POINT('Ctrl Pts',(-14.7614162727808,1.49127933998626,-5.72626316759213));
#29476=CARTESIAN_POINT('Ctrl Pts',(-14.8078358208084,0.53725674277749,-5.97471737716275));
#29477=CARTESIAN_POINT('Ctrl Pts',(-14.854255368836,-0.480205712154302,
-5.97957314685963));
#29478=CARTESIAN_POINT('Ctrl Pts',(-14.9006749168636,-1.43655625981935,
-5.74023606193734));
#29479=CARTESIAN_POINT('Ctrl Pts',(-14.9470944648912,-2.3929068074845,-5.50089897701502));
#29480=CARTESIAN_POINT('Ctrl Pts',(-14.9935140129189,-3.2881454478829,-5.01736903747348));
#29481=CARTESIAN_POINT('Ctrl Pts',(-15.0399335609465,-4.01268233599549,
-4.34883713247367));
#29482=CARTESIAN_POINT('Ctrl Pts',(-15.0863531089741,-4.73721922410796,
-3.68030522747397));
#29483=CARTESIAN_POINT('Ctrl Pts',(-15.1327726570017,-5.29105435993469,
-2.82677135701607));
#29484=CARTESIAN_POINT('Ctrl Pts',(-15.1791922050293,-5.60639050599904,
-1.89272011365545));
#29485=CARTESIAN_POINT('Ctrl Pts',(-15.2094197392846,-5.81173145743218,
-1.28448355913171));
#29486=CARTESIAN_POINT('Ctrl Pts',(-15.2396472735398,-5.91594004170654,
-0.642104669132373));
#29487=CARTESIAN_POINT('Ctrl Pts',(-15.2698748077951,-5.91641904191932,
0.000122539150512468));
#29488=CARTESIAN_POINT('Ctrl Pts',(-15.5216251922048,-5.91631764548591,
8.65724823460925E-5));
#29489=CARTESIAN_POINT('Ctrl Pts',(-15.4938367367167,-5.91601344679757,
-0.59034788972918));
#29490=CARTESIAN_POINT('Ctrl Pts',(-15.4660482812286,-5.82819353340298,
-1.18087085127824));
#29491=CARTESIAN_POINT('Ctrl Pts',(-15.4382598257405,-5.65417516915888,
-1.74479425457244));
#29492=CARTESIAN_POINT('Ctrl Pts',(-15.3918402777129,-5.36348417267047,
-2.68680664940669));
#29493=CARTESIAN_POINT('Ctrl Pts',(-15.3454207296853,-4.83226140010595,
-3.55459452017086));
#29494=CARTESIAN_POINT('Ctrl Pts',(-15.2990011816577,-4.12553601652687,
-4.2419283834904));
#29495=CARTESIAN_POINT('Ctrl Pts',(-15.25258163363,-3.41881063294774,-4.92926224680999));
#29496=CARTESIAN_POINT('Ctrl Pts',(-15.2061620856024,-2.53658263835401,
-5.43614210268493));
#29497=CARTESIAN_POINT('Ctrl Pts',(-15.1597425375748,-1.58684919108548,
-5.7005187026334));
#29498=CARTESIAN_POINT('Ctrl Pts',(-15.1133229895472,-0.6371157438171,-5.96489530258183));
#29499=CARTESIAN_POINT('Ctrl Pts',(-15.0669034415196,0.380123156126065,
-5.98676864660388));
#29500=CARTESIAN_POINT('Ctrl Pts',(-15.020483893492,1.34034311004015,-5.76346112866998));
#29501=CARTESIAN_POINT('Ctrl Pts',(-14.9740643454644,2.30056306395439,-5.54015361073604));
#29502=CARTESIAN_POINT('Ctrl Pts',(-14.9276447974368,3.20376407183954,-5.07166523084607));
#29503=CARTESIAN_POINT('Ctrl Pts',(-14.8812252494091,3.93938158251497,-4.4153455789625));
#29504=CARTESIAN_POINT('Ctrl Pts',(-14.8348057013815,4.67499909319041,-3.75902592707893));
#29505=CARTESIAN_POINT('Ctrl Pts',(-14.7883861533539,5.24303310665613,-2.91487500320176));
#29506=CARTESIAN_POINT('Ctrl Pts',(-14.7419666053263,5.57394824240897,-1.98622879479375));
#29507=CARTESIAN_POINT('Ctrl Pts',(-14.6955470572987,5.9048633781618,-1.05758258638574));
#29508=CARTESIAN_POINT('Ctrl Pts',(-14.6491275092711,5.99865963620174,-0.0444410934468829));
#29509=CARTESIAN_POINT('Ctrl Pts',(-14.6027079612435,5.84385503070052,0.929172865767193));
#29510=CARTESIAN_POINT('Ctrl Pts',(-14.5562884132158,5.68905042519931,1.90278682498127));
#29511=CARTESIAN_POINT('Ctrl Pts',(-14.5098688651882,5.28564495615694,2.83687325047057));
#29512=CARTESIAN_POINT('Ctrl Pts',(-14.4634493171606,4.68302114666527,3.6170867800217));
#29513=CARTESIAN_POINT('Ctrl Pts',(-14.417029769133,4.08039733717367,4.39730030957275));
#29514=CARTESIAN_POINT('Ctrl Pts',(-14.3706102211054,3.27855518723281,5.02364094318566));
#29515=CARTESIAN_POINT('Ctrl Pts',(-14.3241906730778,2.37565149322788,5.41943574710928));
#29516=CARTESIAN_POINT('Ctrl Pts',(-14.2777711250502,1.47274779922286,5.81523055103295));
#29517=CARTESIAN_POINT('Ctrl Pts',(-14.2313515770226,0.468782561153745,
5.98047952526726));
#29518=CARTESIAN_POINT('Ctrl Pts',(-14.1849320289949,-0.513344705833924,
5.89495386303524));
#29519=CARTESIAN_POINT('Ctrl Pts',(-14.1385124809673,-1.49547197282154,
5.80942820080323));
#29520=CARTESIAN_POINT('Ctrl Pts',(-14.0920929329397,-2.45576126872771,
5.47312790210493));
#29521=CARTESIAN_POINT('Ctrl Pts',(-14.0456733849121,-3.27665963017168,
4.92722087005698));
#29522=CARTESIAN_POINT('Ctrl Pts',(-13.9992538368845,-4.09755799161564,
4.38131383800903));
#29523=CARTESIAN_POINT('Ctrl Pts',(-13.9528342888569,-4.77906541859739,
3.62580007261144));
#29524=CARTESIAN_POINT('Ctrl Pts',(-13.9064147408293,-5.23775578323106,
2.75316512210063));
#29525=CARTESIAN_POINT('Ctrl Pts',(-13.8614848912878,-5.68172583345341,
1.90853481661455));
#29526=CARTESIAN_POINT('Ctrl Pts',(-13.8165550417463,-5.91695065499682,
0.954180020948209));
#29527=CARTESIAN_POINT('Ctrl Pts',(-13.7716251922048,-5.91724766713751,
-3.36308197105027E-5));
#29528=CARTESIAN_POINT('Origin',(-29.75,0.,0.));
#29529=CARTESIAN_POINT('',(-11.7698748077951,-5.91624143118648,1.67735000153324E-5));
#29530=CARTESIAN_POINT('',(-12.0216251922048,-5.916248517546,-3.1785587739037E-5));
#29531=CARTESIAN_POINT('',(-29.75,-5.91675,-7.2459289488551E-16));
#29532=CARTESIAN_POINT('Ctrl Pts',(-11.7698748077951,-5.91624143118648,
1.67735000153324E-5));
#29533=CARTESIAN_POINT('Ctrl Pts',(-11.7922447875438,-5.91628813593339,
0.47533983721482));
#29534=CARTESIAN_POINT('Ctrl Pts',(-11.8146147672925,-5.85969045278836,
0.950651967737993));
#29535=CARTESIAN_POINT('Ctrl Pts',(-11.8369847470412,-5.74632229224677,
1.41201418123897));
#29536=CARTESIAN_POINT('Ctrl Pts',(-11.8834042950688,-5.51107403399256,
2.36937872373404));
#29537=CARTESIAN_POINT('Ctrl Pts',(-11.9298238430964,-5.0313740094756,3.26667539272024));
#29538=CARTESIAN_POINT('Ctrl Pts',(-11.976243391124,-4.36594427220227,3.99406241143229));
#29539=CARTESIAN_POINT('Ctrl Pts',(-12.0226629391517,-3.70051453492894,
4.72144943014433));
#29540=CARTESIAN_POINT('Ctrl Pts',(-12.0690824871793,-2.84935508489923,
5.27892679858222));
#29541=CARTESIAN_POINT('Ctrl Pts',(-12.1155020352069,-1.91665985209559,
5.59825141859108));
#29542=CARTESIAN_POINT('Ctrl Pts',(-12.1619215832345,-0.983964619291893,
5.91757603859996));
#29543=CARTESIAN_POINT('Ctrl Pts',(-12.2083411312621,0.0302663962857454,
5.9987479101798));
#29544=CARTESIAN_POINT('Ctrl Pts',(-12.2547606792897,1.00187700343316,5.83183045058615));
#29545=CARTESIAN_POINT('Ctrl Pts',(-12.3011802273173,1.97348761058057,5.6649129909925));
#29546=CARTESIAN_POINT('Ctrl Pts',(-12.3475997753449,2.90247780929775,5.24990620022537));
#29547=CARTESIAN_POINT('Ctrl Pts',(-12.3940193233726,3.67512608745658,4.63761276689723));
#29548=CARTESIAN_POINT('Ctrl Pts',(-12.4404388714002,4.44777436561531,4.02531933356917));
#29549=CARTESIAN_POINT('Ctrl Pts',(-12.4868584194278,5.06408072321573,3.21573925768014));
#29550=CARTESIAN_POINT('Ctrl Pts',(-12.5332779674554,5.44860056351477,2.30797656696481));
#29551=CARTESIAN_POINT('Ctrl Pts',(-12.579697515483,5.83312040381384,1.40021387624937));
#29552=CARTESIAN_POINT('Ctrl Pts',(-12.6261170635106,5.98585372681148,0.394268570707601));
#29553=CARTESIAN_POINT('Ctrl Pts',(-12.6725366115382,5.88810381808847,-0.586717446309564));
#29554=CARTESIAN_POINT('Ctrl Pts',(-12.7189561595658,5.79035390936548,-1.56770346332667));
#29555=CARTESIAN_POINT('Ctrl Pts',(-12.7653757075934,5.44212076892188,-2.52373019181918));
#29556=CARTESIAN_POINT('Ctrl Pts',(-12.8117952556211,4.88603304812455,-3.3377664668198));
#29557=CARTESIAN_POINT('Ctrl Pts',(-12.8582148036487,4.32994532732723,-4.15180274182043));
#29558=CARTESIAN_POINT('Ctrl Pts',(-12.9046343516763,3.56600302617619,-4.82384856332916));
#29559=CARTESIAN_POINT('Ctrl Pts',(-12.9510538997039,2.68772346464476,-5.27163603751151));
#29560=CARTESIAN_POINT('Ctrl Pts',(-12.9974734477315,1.80944390311323,-5.71942351169391));
#29561=CARTESIAN_POINT('Ctrl Pts',(-13.0438929957591,0.816827081201296,
-5.94295263854987));
#29562=CARTESIAN_POINT('Ctrl Pts',(-13.0903125437867,-0.168616692255152,
-5.91486029805312));
#29563=CARTESIAN_POINT('Ctrl Pts',(-13.1367320918144,-1.15406046571149,
-5.88676795755636));
#29564=CARTESIAN_POINT('Ctrl Pts',(-13.183151639842,-2.13233119071233,-5.60705414970694));
#29565=CARTESIAN_POINT('Ctrl Pts',(-13.2295711878696,-2.98367472316512,
-5.10995979247759));
#29566=CARTESIAN_POINT('Ctrl Pts',(-13.2759907358972,-3.8350182556179,-4.61286543524824));
#29567=CARTESIAN_POINT('Ctrl Pts',(-13.3224102839248,-4.55943459552262,
-3.89839052863896));
#29568=CARTESIAN_POINT('Ctrl Pts',(-13.3688298319524,-5.06824495843351,
-3.05399688534637));
#29569=CARTESIAN_POINT('Ctrl Pts',(-13.41524937998,-5.5770553213444,-2.20960324205378));
#29570=CARTESIAN_POINT('Ctrl Pts',(-13.4616689280076,-5.87025970726146,
-1.23529086207788));
#29571=CARTESIAN_POINT('Ctrl Pts',(-13.5080884760353,-5.91196576104991,
-0.250329332211946));
#29572=CARTESIAN_POINT('Ctrl Pts',(-13.5120172532885,-5.91549560574704,
-0.166965865346676));
#29573=CARTESIAN_POINT('Ctrl Pts',(-13.5159460305418,-5.91722389302913,
-0.0835261154508764));
#29574=CARTESIAN_POINT('Ctrl Pts',(-13.5198748077951,-5.91716619296352,
-8.39733533108955E-5));
#29575=CARTESIAN_POINT('Ctrl Pts',(-13.7716251922048,-5.91724766713751,
-3.36308197105027E-5));
#29576=CARTESIAN_POINT('Ctrl Pts',(-13.7701354937187,-5.9172575149011,-0.0316716319925286));
#29577=CARTESIAN_POINT('Ctrl Pts',(-13.7686457952326,-5.91700910022253,
-0.0633094780020733));
#29578=CARTESIAN_POINT('Ctrl Pts',(-13.7671560967464,-5.91650146876277,
-0.0949431643132593));
#29579=CARTESIAN_POINT('Ctrl Pts',(-13.7207365487188,-5.90068348737519,
-1.08066036459218));
#29580=CARTESIAN_POINT('Ctrl Pts',(-13.6743170006912,-5.63317422231444,
-2.06233862952592));
#29581=CARTESIAN_POINT('Ctrl Pts',(-13.6278974526636,-5.14672058326051,
-2.91980668403996));
#29582=CARTESIAN_POINT('Ctrl Pts',(-13.581477904636,-4.66026694420664,-3.7772747385539));
#29583=CARTESIAN_POINT('Ctrl Pts',(-13.5350583566084,-3.95486893115965,
-4.51053258264816));
#29584=CARTESIAN_POINT('Ctrl Pts',(-13.4886388085808,-3.11687721693247,
-5.02981910697483));
#29585=CARTESIAN_POINT('Ctrl Pts',(-13.4422192605532,-2.27888550270521,
-5.54910563130157));
#29586=CARTESIAN_POINT('Ctrl Pts',(-13.3957997125255,-1.30830008729773,
-5.85442083586066));
#29587=CARTESIAN_POINT('Ctrl Pts',(-13.3493801644979,-0.323934324437635,
-5.90838983038297));
#29588=CARTESIAN_POINT('Ctrl Pts',(-13.3029606164703,0.660431438422463,
-5.96235882490529));
#29589=CARTESIAN_POINT('Ctrl Pts',(-13.2565410684427,1.65857754873518,-5.76498160939082));
#29590=CARTESIAN_POINT('Ctrl Pts',(-13.2101215204151,2.54831683472379,-5.34041994080851));
#29591=CARTESIAN_POINT('Ctrl Pts',(-13.1637019723875,3.43805612071233,-4.91585827222623));
#29592=CARTESIAN_POINT('Ctrl Pts',(-13.1172824243599,4.21938858237678,-4.26411215057615));
#29593=CARTESIAN_POINT('Ctrl Pts',(-13.0708628763323,4.79666809865151,-3.46496449991928));
#29594=CARTESIAN_POINT('Ctrl Pts',(-13.0244433283046,5.37394761492623,-2.6658168492624));
#29595=CARTESIAN_POINT('Ctrl Pts',(-12.978023780277,5.74717418581124,-1.71926766959874));
#29596=CARTESIAN_POINT('Ctrl Pts',(-12.9316042322494,5.87065961129535,-0.741187940152418));
#29597=CARTESIAN_POINT('Ctrl Pts',(-12.8851846842218,5.99414503677946,0.236891789293961));
#29598=CARTESIAN_POINT('Ctrl Pts',(-12.8387651361942,5.86788931686263,1.24650206852301));
#29599=CARTESIAN_POINT('Ctrl Pts',(-12.7923455881666,5.50734793364101,2.16405234967687));
#29600=CARTESIAN_POINT('Ctrl Pts',(-12.745926040139,5.14680655041941,3.08160263083068));
#29601=CARTESIAN_POINT('Ctrl Pts',(-12.6995064921114,4.55197950389303,3.90709291390932));
#29602=CARTESIAN_POINT('Ctrl Pts',(-12.6530869440837,3.79568201996964,4.53947153726081));
#29603=CARTESIAN_POINT('Ctrl Pts',(-12.6066673960561,3.03938453604625,5.17185016061231));
#29604=CARTESIAN_POINT('Ctrl Pts',(-12.5602478480285,2.12161661472584,5.61111712423666));
#29605=CARTESIAN_POINT('Ctrl Pts',(-12.5138283000009,1.15472600299149,5.8034999519546));
#29606=CARTESIAN_POINT('Ctrl Pts',(-12.4674087519733,0.187835391257087,
5.99588277967256));
#29607=CARTESIAN_POINT('Ctrl Pts',(-12.4209892039457,-0.828177910891272,
5.9413814714841));
#29608=CARTESIAN_POINT('Ctrl Pts',(-12.3745696559181,-1.76893953521789,
5.64666775674512));
#29609=CARTESIAN_POINT('Ctrl Pts',(-12.3281501078905,-2.70970115954445,
5.35195404200617));
#29610=CARTESIAN_POINT('Ctrl Pts',(-12.2817305598628,-3.57521110604927,
4.81702792071674));
#29611=CARTESIAN_POINT('Ctrl Pts',(-12.2353110118352,-4.25951874143788,
4.10737190009151));
#29612=CARTESIAN_POINT('Ctrl Pts',(-12.1888914638076,-4.94382637682645,
3.39771587946632));
#29613=CARTESIAN_POINT('Ctrl Pts',(-12.14247191578,-5.44693170109882,2.51332995950535));
#29614=CARTESIAN_POINT('Ctrl Pts',(-12.0960523677524,-5.70724752171524,
1.56247545907036));
#29615=CARTESIAN_POINT('Ctrl Pts',(-12.0712433092366,-5.8463740470841,1.05428858643384));
#29616=CARTESIAN_POINT('Ctrl Pts',(-12.0464342507207,-5.91615022215936,
0.527115640388131));
#29617=CARTESIAN_POINT('Ctrl Pts',(-12.0216251922048,-5.916248517546,-3.1785587739037E-5));
#29618=CARTESIAN_POINT('Origin',(-29.75,0.,0.));
#29619=CARTESIAN_POINT('',(-10.0198748077951,-5.91722893930563,5.01660477857623E-5));
#29620=CARTESIAN_POINT('',(-10.2716251922049,-5.91712979830057,9.76190556973378E-5));
#29621=CARTESIAN_POINT('',(-29.75,-5.91675,-7.2459289488551E-16));
#29622=CARTESIAN_POINT('Ctrl Pts',(-10.0198748077951,-5.91722893930563,
5.01660477857623E-5));
#29623=CARTESIAN_POINT('Ctrl Pts',(-10.0221239965182,-5.91725026066663,
0.0478185513098333));
#29624=CARTESIAN_POINT('Ctrl Pts',(-10.0243731852412,-5.91668394546353,
0.0955864297295038));
#29625=CARTESIAN_POINT('Ctrl Pts',(-10.0266223739643,-5.91552682193497,
0.143339992186572));
#29626=CARTESIAN_POINT('Ctrl Pts',(-10.0730419219919,-5.89164569952976,
1.12889481168223));
#29627=CARTESIAN_POINT('Ctrl Pts',(-10.1194614700195,-5.61611475547292,
2.10835186768951));
#29628=CARTESIAN_POINT('Ctrl Pts',(-10.1658810180471,-5.12266286617188,
2.96181179245674));
#29629=CARTESIAN_POINT('Ctrl Pts',(-10.2123005660748,-4.62921097687081,
3.81527171722401));
#29630=CARTESIAN_POINT('Ctrl Pts',(-10.2587201141024,-3.91783814232551,
4.54273451075121));
#29631=CARTESIAN_POINT('Ctrl Pts',(-10.30513966213,-3.0756264378292,5.0551484596714));
#29632=CARTESIAN_POINT('Ctrl Pts',(-10.3515592101576,-2.23341473333289,
5.56756240859159));
#29633=CARTESIAN_POINT('Ctrl Pts',(-10.3979787581852,-1.26036415888558,
5.86492751290477));
#29634=CARTESIAN_POINT('Ctrl Pts',(-10.4443983062128,-0.275589838474683,
5.91084208681991));
#29635=CARTESIAN_POINT('Ctrl Pts',(-10.4908178542404,0.709184481936216,
5.95675666073506));
#29636=CARTESIAN_POINT('Ctrl Pts',(-10.537237402268,1.7056825483107,5.75122070425218));
#29637=CARTESIAN_POINT('Ctrl Pts',(-10.5836569502957,2.59191893271063,5.31939471938756));
#29638=CARTESIAN_POINT('Ctrl Pts',(-10.6300764983233,3.47815531711046,4.88756873452299));
#29639=CARTESIAN_POINT('Ctrl Pts',(-10.6764960463509,4.25413001953575,4.22945272127673));
#29640=CARTESIAN_POINT('Ctrl Pts',(-10.7229155943785,4.82485278427143,3.42560936834607));
#29641=CARTESIAN_POINT('Ctrl Pts',(-10.7693351424061,5.39557554900716,2.62176601541532));
#29642=CARTESIAN_POINT('Ctrl Pts',(-10.8157546904337,5.76104637605323,1.67219532280013));
#29643=CARTESIAN_POINT('Ctrl Pts',(-10.8621742384613,5.87652647790919,0.693138145555667));
#29644=CARTESIAN_POINT('Ctrl Pts',(-10.908593786489,5.99200657976514,-0.285919031688796));
#29645=CARTESIAN_POINT('Ctrl Pts',(-10.9550133345166,5.857495956431,-1.29446269356253));
#29646=CARTESIAN_POINT('Ctrl Pts',(-11.0014328825442,5.48946060669121,-2.20903286122626));
#29647=CARTESIAN_POINT('Ctrl Pts',(-11.0478524305718,5.12142525695144,-3.12360302888994));
#29648=CARTESIAN_POINT('Ctrl Pts',(-11.0942719785994,4.51986518080605,-3.94419970234363));
#29649=CARTESIAN_POINT('Ctrl Pts',(-11.140691526627,3.75841982201842,-4.57037026682205));
#29650=CARTESIAN_POINT('Ctrl Pts',(-11.1871110746546,2.99697446323079,-5.19654083130047));
#29651=CARTESIAN_POINT('Ctrl Pts',(-11.2335306226822,2.07564382180092,-5.62828528680363));
#29652=CARTESIAN_POINT('Ctrl Pts',(-11.2799501707098,1.10721177193765,-5.81275201831927));
#29653=CARTESIAN_POINT('Ctrl Pts',(-11.3263697187375,0.138779722074373,
-5.99721874983492));
#29654=CARTESIAN_POINT('Ctrl Pts',(-11.3727892667651,-0.8767537362223,-5.93440775736305));
#29655=CARTESIAN_POINT('Ctrl Pts',(-11.4192088147927,-1.81507297437667,
-5.63200799289912));
#29656=CARTESIAN_POINT('Ctrl Pts',(-11.4656283628203,-2.75339221253104,
-5.32960822843518));
#29657=CARTESIAN_POINT('Ctrl Pts',(-11.5120479108479,-3.61449723054312,
-4.78761969197916));
#29658=CARTESIAN_POINT('Ctrl Pts',(-11.5584674588755,-4.29297662053726,
-4.07238943004136));
#29659=CARTESIAN_POINT('Ctrl Pts',(-11.6048870069031,-4.97145601053144,
-3.35715916810351));
#29660=CARTESIAN_POINT('Ctrl Pts',(-11.6513065549308,-5.46730977250767,
-2.46868718068385));
#29661=CARTESIAN_POINT('Ctrl Pts',(-11.6977261029584,-5.71983840750006,
-1.51573497897201));
#29662=CARTESIAN_POINT('Ctrl Pts',(-11.7217756712373,-5.85067131966066,
-1.02201864575865));
#29663=CARTESIAN_POINT('Ctrl Pts',(-11.7458252395162,-5.91619121974183,
-0.510994617827731));
#29664=CARTESIAN_POINT('Ctrl Pts',(-11.7698748077951,-5.91624143118648,
1.67735000153324E-5));
#29665=CARTESIAN_POINT('Ctrl Pts',(-12.0216251922048,-5.916248517546,-3.1785587739037E-5));
#29666=CARTESIAN_POINT('Ctrl Pts',(-12.0000147026931,-5.9163341399577,-0.459215430663503));
#29667=CARTESIAN_POINT('Ctrl Pts',(-11.9784042131813,-5.86355046136694,
-0.918379711943183));
#29668=CARTESIAN_POINT('Ctrl Pts',(-11.9567937236695,-5.75768100403336,
-1.36495908001494));
#29669=CARTESIAN_POINT('Ctrl Pts',(-11.9103741756419,-5.53027234877463,
-2.32421603775583));
#29670=CARTESIAN_POINT('Ctrl Pts',(-11.8639546276143,-5.05792872129679,
-3.22540687232847));
#29671=CARTESIAN_POINT('Ctrl Pts',(-11.8175350795867,-4.39847164828013,
-3.95821310613738));
#29672=CARTESIAN_POINT('Ctrl Pts',(-11.7711155315591,-3.73901457526351,
-4.69101933994624));
#29673=CARTESIAN_POINT('Ctrl Pts',(-11.7246959835315,-2.89244405670809,
-5.25544097299139));
#29674=CARTESIAN_POINT('Ctrl Pts',(-11.6782764355039,-1.9623922726155,-5.5823848311184));
#29675=CARTESIAN_POINT('Ctrl Pts',(-11.6318568874763,-1.03234048852291,
-5.90932868924541));
#29676=CARTESIAN_POINT('Ctrl Pts',(-11.5854373394486,-0.0188074388931536,
-5.99879477245428));
#29677=CARTESIAN_POINT('Ctrl Pts',(-11.539017791421,0.954136125952757,-5.83983116943235));
#29678=CARTESIAN_POINT('Ctrl Pts',(-11.4925982433934,1.92707969079872,-5.68086756641042));
#29679=CARTESIAN_POINT('Ctrl Pts',(-11.4461786953658,2.85943377086084,-5.27347427715765));
#29680=CARTESIAN_POINT('Ctrl Pts',(-11.3997591473382,3.63706506745639,-4.66752199024389));
#29681=CARTESIAN_POINT('Ctrl Pts',(-11.3533395993106,4.41469636405186,-4.06156970333021));
#29682=CARTESIAN_POINT('Ctrl Pts',(-11.306920051283,5.03760487718081,-3.25705841875559));
#29683=CARTESIAN_POINT('Ctrl Pts',(-11.2605005032554,5.42953781308038,-2.35247167265668));
#29684=CARTESIAN_POINT('Ctrl Pts',(-11.2140809552277,5.82147074898,-1.44788492655767));
#29685=CARTESIAN_POINT('Ctrl Pts',(-11.1676614072001,5.9824281076502,-0.44322271893434));
#29686=CARTESIAN_POINT('Ctrl Pts',(-11.1212418591725,5.89270643663109,0.538530116157276));
#29687=CARTESIAN_POINT('Ctrl Pts',(-11.0748223111449,5.80298476561198,1.52028295124889));
#29688=CARTESIAN_POINT('Ctrl Pts',(-11.0284027631173,5.46258406490356,2.4791264138088));
#29689=CARTESIAN_POINT('Ctrl Pts',(-10.9819832150897,4.91317418470176,3.29768453086436));
#29690=CARTESIAN_POINT('Ctrl Pts',(-10.9355636670621,4.36376430449999,4.11624264791987));
#29691=CARTESIAN_POINT('Ctrl Pts',(-10.8891441190345,3.60534524480486,4.79451541947105));
#29692=CARTESIAN_POINT('Ctrl Pts',(-10.8427245710069,2.73075820288027,5.24947268511076));
#29693=CARTESIAN_POINT('Ctrl Pts',(-10.7963050229792,1.85617116095567,5.70442995075048));
#29694=CARTESIAN_POINT('Ctrl Pts',(-10.7498854749516,0.865416136801603,
5.93607171047874));
#29695=CARTESIAN_POINT('Ctrl Pts',(-10.703465926924,-0.120224471069116,
5.91604174350367));
#29696=CARTESIAN_POINT('Ctrl Pts',(-10.6570463788964,-1.10586507893989,
5.8960117765286));
#29697=CARTESIAN_POINT('Ctrl Pts',(-10.6106268308688,-2.08639127052732,
5.62431008285018));
#29698=CARTESIAN_POINT('Ctrl Pts',(-10.5642072828412,-2.94177280079486,
5.13419678458329));
#29699=CARTESIAN_POINT('Ctrl Pts',(-10.5177877348136,-3.79715433106241,
4.64408348631641));
#29700=CARTESIAN_POINT('Ctrl Pts',(-10.471368186786,-4.52739120001007,3.93555858346107));
#29701=CARTESIAN_POINT('Ctrl Pts',(-10.4249486387583,-5.04309210828604,
3.09535552427583));
#29702=CARTESIAN_POINT('Ctrl Pts',(-10.3785290907307,-5.55879301656195,
2.25515246509068));
#29703=CARTESIAN_POINT('Ctrl Pts',(-10.3321095427031,-5.85995796416621,
1.28327124957567));
#29704=CARTESIAN_POINT('Ctrl Pts',(-10.2856899946755,-5.90972011085785,
0.298683855680485));
#29705=CARTESIAN_POINT('Ctrl Pts',(-10.2810017271853,-5.91474597311827,
0.199242795476116));
#29706=CARTESIAN_POINT('Ctrl Pts',(-10.2763134596951,-5.91720739231159,
0.0996721254546018));
#29707=CARTESIAN_POINT('Ctrl Pts',(-10.2716251922049,-5.91712979830057,
9.76190556973378E-5));
#29708=CARTESIAN_POINT('Origin',(-29.75,0.,0.));
#29709=CARTESIAN_POINT('',(-8.26987480779513,-5.91634522401586,-9.88515524452672E-5));
#29710=CARTESIAN_POINT('',(-8.52162519220486,-5.9164576885749,-0.000131435617752113));
#29711=CARTESIAN_POINT('',(-29.75,-5.91675,-7.2459289488551E-16));
#29712=CARTESIAN_POINT('Ctrl Pts',(-8.26987480779513,-5.91634522401586,
-9.88515524452672E-5));
#29713=CARTESIAN_POINT('Ctrl Pts',(-8.29842275352017,-5.91598626571606,
0.606464769270553));
#29714=CARTESIAN_POINT('Ctrl Pts',(-8.32697069924521,-5.82322044315546,
1.21313569281818));
#29715=CARTESIAN_POINT('Ctrl Pts',(-8.35551864497026,-5.63971267484951,
1.7909899160894));
#29716=CARTESIAN_POINT('Ctrl Pts',(-8.40193819299787,-5.34132526209617,
2.73059279079175));
#29717=CARTESIAN_POINT('Ctrl Pts',(-8.4483577410255,-4.80302131586862,3.59400595212951));
#29718=CARTESIAN_POINT('Ctrl Pts',(-8.49477728905311,-4.0906968368287,4.27553544290674));
#29719=CARTESIAN_POINT('Ctrl Pts',(-8.54119683708072,-3.37837235778882,
4.95706493368393));
#29720=CARTESIAN_POINT('Ctrl Pts',(-8.58761638510832,-2.49202734593661,
5.45671075390062));
#29721=CARTESIAN_POINT('Ctrl Pts',(-8.63403593313593,-1.54016294063202,
5.71330920314101));
#29722=CARTESIAN_POINT('Ctrl Pts',(-8.68045548116354,-0.588298535327425,
5.96990765238141));
#29723=CARTESIAN_POINT('Ctrl Pts',(-8.72687502919116,0.429085263429556,
5.98345873064552));
#29724=CARTESIAN_POINT('Ctrl Pts',(-8.77329457721878,1.3874463192751,5.75230359469335));
#29725=CARTESIAN_POINT('Ctrl Pts',(-8.81971412524639,2.34580737512064,5.52114845874118));
#29726=CARTESIAN_POINT('Ctrl Pts',(-8.86613367327399,3.24514568805474,5.04528710857274));
#29727=CARTESIAN_POINT('Ctrl Pts',(-8.91255322130161,3.97536955527705,4.38297168977492));
#29728=CARTESIAN_POINT('Ctrl Pts',(-8.95897276932922,4.70559342249941,3.72065627097706));
#29729=CARTESIAN_POINT('Ctrl Pts',(-9.00539231735684,5.26670284400996,2.8718867835498));
#29730=CARTESIAN_POINT('Ctrl Pts',(-9.05181186538445,5.5900101070948,1.94056459232104));
#29731=CARTESIAN_POINT('Ctrl Pts',(-9.09823141341206,5.91331737017962,1.00924240109232));
#29732=CARTESIAN_POINT('Ctrl Pts',(-9.14465096143967,5.99882247483874,-0.00463249393789208));
#29733=CARTESIAN_POINT('Ctrl Pts',(-9.19107050946728,5.83605838943942,-0.976947495746754));
#29734=CARTESIAN_POINT('Ctrl Pts',(-9.23749005749489,5.67329430404009,-1.94926249755562));
#29735=CARTESIAN_POINT('Ctrl Pts',(-9.28390960552251,5.26226102858231,-2.88001760614312));
#29736=CARTESIAN_POINT('Ctrl Pts',(-9.33032915355012,4.65327483732233,-3.65527525950303));
#29737=CARTESIAN_POINT('Ctrl Pts',(-9.37674870157774,4.04428864606231,-4.43053291286298));
#29738=CARTESIAN_POINT('Ctrl Pts',(-9.42316824960535,3.23734953900007,-5.05029311099531));
#29739=CARTESIAN_POINT('Ctrl Pts',(-9.46958779763296,2.33123825201114,-5.43868845832818));
#29740=CARTESIAN_POINT('Ctrl Pts',(-9.51600734566057,1.42512696502221,-5.82708380566105));
#29741=CARTESIAN_POINT('Ctrl Pts',(-9.56242689368819,0.419843498106589,
-5.98411430219445));
#29742=CARTESIAN_POINT('Ctrl Pts',(-9.6088464417158,-0.561551263773847,
-5.89055719881796));
#29743=CARTESIAN_POINT('Ctrl Pts',(-9.65526598974341,-1.54294602565423,
-5.79700009544146));
#29744=CARTESIAN_POINT('Ctrl Pts',(-9.70168553777102,-2.50045208249942,
-5.45285539215509));
#29745=CARTESIAN_POINT('Ctrl Pts',(-9.74810508579863,-3.31685717867248,
-4.90025125791331));
#29746=CARTESIAN_POINT('Ctrl Pts',(-9.79452463382625,-4.13326227484553,
-4.34764712367153));
#29747=CARTESIAN_POINT('Ctrl Pts',(-9.84094418185386,-4.80856641034645,
-3.58658355847433));
#29748=CARTESIAN_POINT('Ctrl Pts',(-9.88736372988147,-5.26010282772011,
-2.71022548438372));
#29749=CARTESIAN_POINT('Ctrl Pts',(-9.93153408918603,-5.68976073353647,
-1.87633001023987));
#29750=CARTESIAN_POINT('Ctrl Pts',(-9.97570444849058,-5.91681022291855,
-0.938042186448962));
#29751=CARTESIAN_POINT('Ctrl Pts',(-10.0198748077951,-5.91722893930563,
5.01660477857623E-5));
#29752=CARTESIAN_POINT('Ctrl Pts',(-10.2716251922049,-5.91712979830057,
9.76190556973378E-5));
#29753=CARTESIAN_POINT('Ctrl Pts',(-10.2298939116675,-5.91643911726574,
-0.886236548007039));
#29754=CARTESIAN_POINT('Ctrl Pts',(-10.1881626311301,-5.71457825033594,
-1.7728746775507));
#29755=CARTESIAN_POINT('Ctrl Pts',(-10.1464313505927,-5.3294818102357,-2.5711140520577));
#29756=CARTESIAN_POINT('Ctrl Pts',(-10.1000118025651,-4.90112201714299,
-3.45903099362507));
#29757=CARTESIAN_POINT('Ctrl Pts',(-10.0535922545374,-4.24604308517861,
-4.2375713044844));
#29758=CARTESIAN_POINT('Ctrl Pts',(-10.0071727065098,-3.44443592142545,
-4.81143066223716));
#29759=CARTESIAN_POINT('Ctrl Pts',(-9.96075315848222,-2.64282875767234,
-5.38529001998988));
#29760=CARTESIAN_POINT('Ctrl Pts',(-9.91433361045461,-1.69469336213048,
-5.75446842463606));
#29761=CARTESIAN_POINT('Ctrl Pts',(-9.867914062427,-0.716094889235394,-5.87377322884811));
#29762=CARTESIAN_POINT('Ctrl Pts',(-9.82149451439938,0.26250358365986,-5.99307803306019));
#29763=CARTESIAN_POINT('Ctrl Pts',(-9.77507496637177,1.27156513390835,-5.86250923683805));
#29764=CARTESIAN_POINT('Ctrl Pts',(-9.72865541834415,2.18756638582422,-5.49805030369255));
#29765=CARTESIAN_POINT('Ctrl Pts',(-9.68223587031654,3.10356763774005,-5.13359137054708));
#29766=CARTESIAN_POINT('Ctrl Pts',(-9.63581632228892,3.92650859132326,-4.53524230047826));
#29767=CARTESIAN_POINT('Ctrl Pts',(-9.58939677426131,4.55564965883346,-3.77624946478545));
#29768=CARTESIAN_POINT('Ctrl Pts',(-9.5429772262337,5.18479072634363,-3.01725662909268));
#29769=CARTESIAN_POINT('Ctrl Pts',(-9.49655767820609,5.62013190778081,-2.09762002777593));
#29770=CARTESIAN_POINT('Ctrl Pts',(-9.45013813017848,5.80838129811409,-1.12991616062445));
#29771=CARTESIAN_POINT('Ctrl Pts',(-9.40371858215087,5.99663068844738,-0.162212293472971));
#29772=CARTESIAN_POINT('Ctrl Pts',(-9.35729903412325,5.93778828767677,0.853558839513239));
#29773=CARTESIAN_POINT('Ctrl Pts',(-9.31087948609563,5.63905723616061,1.79305251502193));
#29774=CARTESIAN_POINT('Ctrl Pts',(-9.26445993806802,5.34032618464443,2.73254619053068));
#29775=CARTESIAN_POINT('Ctrl Pts',(-9.21804039004041,4.80170648238268,3.5957624085619));
#29776=CARTESIAN_POINT('Ctrl Pts',(-9.1716208420128,4.08913278303239,4.27703132056005));
#29777=CARTESIAN_POINT('Ctrl Pts',(-9.12520129398519,3.37655908368215,4.95830023255815));
#29778=CARTESIAN_POINT('Ctrl Pts',(-9.07878174595758,2.49003138724338,5.45762183852321));
#29779=CARTESIAN_POINT('Ctrl Pts',(-9.03236219792996,1.53807319624787,5.7138721264398));
#29780=CARTESIAN_POINT('Ctrl Pts',(-8.98594264990235,0.586115005252362,
5.9701224143564));
#29781=CARTESIAN_POINT('Ctrl Pts',(-8.93952310187473,-0.431273680299897,
5.98330138422453));
#29782=CARTESIAN_POINT('Ctrl Pts',(-8.89310355384712,-1.38955012583237,
5.75179574412384));
#29783=CARTESIAN_POINT('Ctrl Pts',(-8.84668400581951,-2.3478265713649,5.52029010402313));
#29784=CARTESIAN_POINT('Ctrl Pts',(-8.8002644577919,-3.24699077687763,5.04409985395356));
#29785=CARTESIAN_POINT('Ctrl Pts',(-8.75384490976429,-3.97697235277594,
4.38151740149205));
#29786=CARTESIAN_POINT('Ctrl Pts',(-8.70742536173668,-4.70695392867421,
3.71893494903058));
#29787=CARTESIAN_POINT('Ctrl Pts',(-8.66100581370906,-5.26775287495808,
2.86996029417718));
#29788=CARTESIAN_POINT('Ctrl Pts',(-8.61458626568145,-5.59071948546345,
1.93851991714843));
#29789=CARTESIAN_POINT('Ctrl Pts',(-8.58359924118925,-5.80631344738524,
1.31674381198596));
#29790=CARTESIAN_POINT('Ctrl Pts',(-8.55261221669705,-5.91592620827154,
0.658219901896991));
#29791=CARTESIAN_POINT('Ctrl Pts',(-8.52162519220486,-5.9164576885749,-0.000131435617752112));
#29792=CARTESIAN_POINT('Origin',(-29.75,0.,0.));
#29793=CARTESIAN_POINT('',(-6.51987480779513,-5.91690427471314,0.000144985681112611));
#29794=CARTESIAN_POINT('',(-6.77162519220487,-5.916739287675,0.000155466350801038));
#29795=CARTESIAN_POINT('',(-29.75,-5.91675,-7.2459289488551E-16));
#29796=CARTESIAN_POINT('Ctrl Pts',(-6.51987480779513,-5.91690427471314,
0.000144985681112611));
#29797=CARTESIAN_POINT('Ctrl Pts',(-6.52830196249454,-5.91708722319681,
0.179149749583483));
#29798=CARTESIAN_POINT('Ctrl Pts',(-6.53672911719395,-5.9091261911554,0.35813830044998));
#29799=CARTESIAN_POINT('Ctrl Pts',(-6.54515627189336,-5.89290301795475,
0.536374827309976));
#29800=CARTESIAN_POINT('Ctrl Pts',(-6.59157581992097,-5.80354042827781,
1.51816041378229));
#29801=CARTESIAN_POINT('Ctrl Pts',(-6.63799536794859,-5.46349044623204,
2.47712831491668));
#29802=CARTESIAN_POINT('Ctrl Pts',(-6.68441491597621,-4.91437998909899,
3.29588732470264));
#29803=CARTESIAN_POINT('Ctrl Pts',(-6.73083446400383,-4.36526953196594,
4.1146463344886));
#29804=CARTESIAN_POINT('Ctrl Pts',(-6.77725401203144,-3.60709859974563,
4.79319645292615));
#29805=CARTESIAN_POINT('Ctrl Pts',(-6.82367356005905,-2.73267801539693,
5.24847356843477));
#29806=CARTESIAN_POINT('Ctrl Pts',(-6.87009310808666,-1.85825743104829,
5.70375068394336));
#29807=CARTESIAN_POINT('Ctrl Pts',(-6.91651265611427,-0.867587194571285,
5.93575479652306));
#29808=CARTESIAN_POINT('Ctrl Pts',(-6.96293220414188,0.118060674729629,
5.9160853282787));
#29809=CARTESIAN_POINT('Ctrl Pts',(-7.00935175216949,1.10370854403049,5.89641586003434));
#29810=CARTESIAN_POINT('Ctrl Pts',(-7.0557713001971,2.08433404615525,5.62507281096596));
#29811=CARTESIAN_POINT('Ctrl Pts',(-7.10219084822471,2.93989477905598,5.13527240002626));
#29812=CARTESIAN_POINT('Ctrl Pts',(-7.14861039625233,3.79545551195686,4.64547198908647));
#29813=CARTESIAN_POINT('Ctrl Pts',(-7.19502994427994,4.52595147563366,3.93721421627529));
#29814=CARTESIAN_POINT('Ctrl Pts',(-7.24144949230756,5.04195965388283,3.09719982936359));
#29815=CARTESIAN_POINT('Ctrl Pts',(-7.28786904033517,5.55796783213196,2.25718544245194));
#29816=CARTESIAN_POINT('Ctrl Pts',(-7.33428858836279,5.8594882249535,1.28541444143978));
#29817=CARTESIAN_POINT('Ctrl Pts',(-7.3807081363904,5.90961048059508,0.300845312466115));
#29818=CARTESIAN_POINT('Ctrl Pts',(-7.42712768441801,5.95973273623666,-0.683723816507492));
#29819=CARTESIAN_POINT('Ctrl Pts',(-7.47354723244562,5.75845685469833,-1.6810910734426));
#29820=CARTESIAN_POINT('Ctrl Pts',(-7.51996678047324,5.33042184469627,-2.56916462920867));
#29821=CARTESIAN_POINT('Ctrl Pts',(-7.56638632850085,4.90238683469421,-3.45723818497473));
#29822=CARTESIAN_POINT('Ctrl Pts',(-7.61280587652846,4.24759269622844,-4.23601803957176));
#29823=CARTESIAN_POINT('Ctrl Pts',(-7.65922542455607,3.44619547363803,-4.81017054706679));
#29824=CARTESIAN_POINT('Ctrl Pts',(-7.70564497258368,2.64479825104767,-5.38432305456179));
#29825=CARTESIAN_POINT('Ctrl Pts',(-7.75206452061129,1.6967979443327,-5.75384821495482));
#29826=CARTESIAN_POINT('Ctrl Pts',(-7.79848406863889,0.718243171149578,
-5.87351093312076));
#29827=CARTESIAN_POINT('Ctrl Pts',(-7.84490361666651,-0.260311602033657,
-5.99317365128671));
#29828=CARTESIAN_POINT('Ctrl Pts',(-7.89132316469413,-1.26942084168505,
-5.86297392722552));
#29829=CARTESIAN_POINT('Ctrl Pts',(-7.93774271272174,-2.18555533426276,
-5.49885004480643));
#29830=CARTESIAN_POINT('Ctrl Pts',(-7.98416226074936,-3.10168982684046,
-5.13472616238734));
#29831=CARTESIAN_POINT('Ctrl Pts',(-8.03058180877697,-3.92484957234447,
-4.53667812161035));
#29832=CARTESIAN_POINT('Ctrl Pts',(-8.07700135680458,-4.55426819981524,
-3.77791544354075));
#29833=CARTESIAN_POINT('Ctrl Pts',(-8.1234209048322,-5.18368682728602,-3.01915276547114));
#29834=CARTESIAN_POINT('Ctrl Pts',(-8.16984045285981,-5.61936433672356,
-2.09967545010891));
#29835=CARTESIAN_POINT('Ctrl Pts',(-8.21626000088743,-5.80796765180276,
-1.13204049839432));
#29836=CARTESIAN_POINT('Ctrl Pts',(-8.23413160319,-5.88058023816478,-0.75949945122988));
#29837=CARTESIAN_POINT('Ctrl Pts',(-8.25200320549256,-5.91656993930847,
-0.379820177456627));
#29838=CARTESIAN_POINT('Ctrl Pts',(-8.26987480779513,-5.91634522401586,
-9.88515524452672E-5));
#29839=CARTESIAN_POINT('Ctrl Pts',(-8.52162519220486,-5.9164576885749,-0.000131435617752112));
#29840=CARTESIAN_POINT('Ctrl Pts',(-8.50619266866945,-5.91672238266621,
-0.328011336229925));
#29841=CARTESIAN_POINT('Ctrl Pts',(-8.49076014513403,-5.88993102800002,
-0.655848432687641));
#29842=CARTESIAN_POINT('Ctrl Pts',(-8.47532762159862,-5.83570067282893,
-0.979081963609703));
#29843=CARTESIAN_POINT('Ctrl Pts',(-8.42890807357101,-5.67258097496215,
-1.95133736813505));
#29844=CARTESIAN_POINT('Ctrl Pts',(-8.38248852554339,-5.26120730450169,
-2.88194207798159));
#29845=CARTESIAN_POINT('Ctrl Pts',(-8.33606897751578,-4.65193760485649,
-3.65697694207167));
#29846=CARTESIAN_POINT('Ctrl Pts',(-8.28964942948816,-4.04266790521129,
-4.43201180616177));
#29847=CARTESIAN_POINT('Ctrl Pts',(-8.24322988146054,-3.23550217638136,
-5.05147682449541));
#29848=CARTESIAN_POINT('Ctrl Pts',(-8.19681033343293,-2.32924889594513,
-5.43954073567431));
#29849=CARTESIAN_POINT('Ctrl Pts',(-8.15039078540532,-1.42299561550895,
-5.82760464685319));
#29850=CARTESIAN_POINT('Ctrl Pts',(-8.10397123737771,-0.417654783466492,
-5.98426745087736));
#29851=CARTESIAN_POINT('Ctrl Pts',(-8.0575516893501,0.563705692919205,-5.89035140938912));
#29852=CARTESIAN_POINT('Ctrl Pts',(-8.01113214132249,1.5450661693049,-5.79643536790087));
#29853=CARTESIAN_POINT('Ctrl Pts',(-7.96471259329487,2.50244629003383,-5.45194048090022));
#29854=CARTESIAN_POINT('Ctrl Pts',(-7.91829304526726,3.31864921582715,-4.89903778477077));
#29855=CARTESIAN_POINT('Ctrl Pts',(-7.87187349723965,4.13485214162051,-4.34613508864129));
#29856=CARTESIAN_POINT('Ctrl Pts',(-7.82545394921204,4.80987787247824,-3.58482458338298));
#29857=CARTESIAN_POINT('Ctrl Pts',(-7.77903440118442,5.26109373160295,-2.70830142000666));
#29858=CARTESIAN_POINT('Ctrl Pts',(-7.73261485315681,5.71230959072763,-1.83177825663038));
#29859=CARTESIAN_POINT('Ctrl Pts',(-7.6861953051292,5.93971557811932,-0.840042435136087));
#29860=CARTESIAN_POINT('Ctrl Pts',(-7.63977575710159,5.91547399130399,0.145503582525929));
#29861=CARTESIAN_POINT('Ctrl Pts',(-7.59335620907397,5.89123240448867,1.13104960018795));
#29862=CARTESIAN_POINT('Ctrl Pts',(-7.54693666104636,5.61534324346633,2.11040581401769));
#29863=CARTESIAN_POINT('Ctrl Pts',(-7.50051711301874,5.12157923545686,2.9636852007693));
#29864=CARTESIAN_POINT('Ctrl Pts',(-7.45409756499113,4.62781522744736,3.81696458752096));
#29865=CARTESIAN_POINT('Ctrl Pts',(-7.40767801696354,3.91617637245083,4.54416714719437));
#29866=CARTESIAN_POINT('Ctrl Pts',(-7.36125846893592,3.07377731041813,5.05627302271945));
#29867=CARTESIAN_POINT('Ctrl Pts',(-7.31483892090831,2.23137824838549,5.56837889824451));
#29868=CARTESIAN_POINT('Ctrl Pts',(-7.26841937288069,1.25821897931661,5.86538808962119));
#29869=CARTESIAN_POINT('Ctrl Pts',(-7.22199982485307,0.273427932955036,
5.91094247982517));
#29870=CARTESIAN_POINT('Ctrl Pts',(-7.17558027682546,-0.71136311340654,
5.95649687002916));
#29871=CARTESIAN_POINT('Ctrl Pts',(-7.12916072879785,-1.70778593706098,
5.75059645906052));
#29872=CARTESIAN_POINT('Ctrl Pts',(-7.08274118077024,-2.59386432084106,
5.31844636330852));
#29873=CARTESIAN_POINT('Ctrl Pts',(-7.03632163274263,-3.47994270462119,
4.88629626755649));
#29874=CARTESIAN_POINT('Ctrl Pts',(-6.98990208471501,-4.25567664852695,
4.22789648702108));
#29875=CARTESIAN_POINT('Ctrl Pts',(-6.9434825366874,-4.82610536908409,3.42384444752088));
#29876=CARTESIAN_POINT('Ctrl Pts',(-6.89706298865978,-5.39653408964123,
2.61979240802068));
#29877=CARTESIAN_POINT('Ctrl Pts',(-6.85064344063217,-5.76165758684977,
1.67008810955569));
#29878=CARTESIAN_POINT('Ctrl Pts',(-6.80422389260456,-5.87677959128358,
0.690988762422807));
#29879=CARTESIAN_POINT('Ctrl Pts',(-6.793357659138,-5.90372820734017,0.46179389635958));
#29880=CARTESIAN_POINT('Ctrl Pts',(-6.78249142567143,-5.9169775084423,0.23098827179514));
#29881=CARTESIAN_POINT('Ctrl Pts',(-6.77162519220487,-5.916739287675,0.000155466350801038));
#29882=CARTESIAN_POINT('Origin',(-29.75,0.,0.));
#29883=CARTESIAN_POINT('',(-4.76987480779513,-5.91668395451438,-0.000155206356347026));
#29884=CARTESIAN_POINT('',(-5.02162519220488,-5.91684860187072,-0.000150428407648674));
#29885=CARTESIAN_POINT('',(-29.75,-5.91675,-7.2459289488551E-16));
#29886=CARTESIAN_POINT('Ctrl Pts',(-4.76987480779513,-5.91668395451438,
-0.000155206356347026));
#29887=CARTESIAN_POINT('Ctrl Pts',(-4.80460071949653,-5.9159368893773,0.737551676700471));
#29888=CARTESIAN_POINT('Ctrl Pts',(-4.83932663119792,-5.77760472280962,
1.47553084454169));
#29889=CARTESIAN_POINT('Ctrl Pts',(-4.87405254289932,-5.50813907390267,
2.16203789905239));
#29890=CARTESIAN_POINT('Ctrl Pts',(-4.92047209092693,-5.14793330770747,
3.07971998792533));
#29891=CARTESIAN_POINT('Ctrl Pts',(-4.96689163895454,-4.553408222658,3.90542777458002));
#29892=CARTESIAN_POINT('Ctrl Pts',(-5.01331118698216,-3.79734208031535,
4.53808297185698));
#29893=CARTESIAN_POINT('Ctrl Pts',(-5.05973073500977,-3.04127593797266,
5.17073816913398));
#29894=CARTESIAN_POINT('Ctrl Pts',(-5.10615028303738,-2.12366873833678,
5.61034077703322));
#29895=CARTESIAN_POINT('Ctrl Pts',(-5.15256983106499,-1.15684855378816,
5.80307723177887));
#29896=CARTESIAN_POINT('Ctrl Pts',(-5.1989893790926,-0.190028369239583,
5.99581368652452));
#29897=CARTESIAN_POINT('Ctrl Pts',(-5.24540892712022,0.826004800221705,
5.94168398811661));
#29898=CARTESIAN_POINT('Ctrl Pts',(-5.29182847514783,1.76687415432054,5.64731437562902));
#29899=CARTESIAN_POINT('Ctrl Pts',(-5.33824802317544,2.70774350841938,5.35294476314143));
#29900=CARTESIAN_POINT('Ctrl Pts',(-5.38466757120306,3.57344904715588,4.81833523657406));
#29901=CARTESIAN_POINT('Ctrl Pts',(-5.43108711923068,4.25801619398554,4.10892954747936));
#29902=CARTESIAN_POINT('Ctrl Pts',(-5.47750666725829,4.94258334081521,3.39952385838465));
#29903=CARTESIAN_POINT('Ctrl Pts',(-5.5239262152859,5.44601209573819,2.51532200676252));
#29904=CARTESIAN_POINT('Ctrl Pts',(-5.5703457633135,5.70667567373816,1.56456277891212));
#29905=CARTESIAN_POINT('Ctrl Pts',(-5.61676531134112,5.96733925173814,0.613803551061655));
#29906=CARTESIAN_POINT('Ctrl Pts',(-5.66318485936872,5.9852376528151,-0.403513053016923));
#29907=CARTESIAN_POINT('Ctrl Pts',(-5.70960440739634,5.75817986005846,-1.36285312253713));
#29908=CARTESIAN_POINT('Ctrl Pts',(-5.75602395542395,5.53112206730183,-2.32219319205729));
#29909=CARTESIAN_POINT('Ctrl Pts',(-5.80244350345158,5.05910808071154,-3.22355672701905));
#29910=CARTESIAN_POINT('Ctrl Pts',(-5.84886305147919,4.39991907427081,-3.95660410886154));
#29911=CARTESIAN_POINT('Ctrl Pts',(-5.89528259950681,3.74073006782999,-4.68965149070412));
#29912=CARTESIAN_POINT('Ctrl Pts',(-5.94170214753442,2.89436604153866,-5.25438271942753));
#29913=CARTESIAN_POINT('Ctrl Pts',(-5.98812169556203,1.96443389783085,-5.58166672199668));
#29914=CARTESIAN_POINT('Ctrl Pts',(-6.03454124358964,1.03450175412321,-5.90895072456578));
#29915=CARTESIAN_POINT('Ctrl Pts',(-6.08096079161725,0.0210014929991525,
-5.99878750098069));
#29916=CARTESIAN_POINT('Ctrl Pts',(-6.12738033964486,-0.952000148996213,
-5.84017976184837));
#29917=CARTESIAN_POINT('Ctrl Pts',(-6.17379988767247,-1.92500179099163,
-5.68157202271603));
#29918=CARTESIAN_POINT('Ctrl Pts',(-6.22021943570009,-2.85750481385833,
-5.27451976803642));
#29919=CARTESIAN_POINT('Ctrl Pts',(-6.2666389837277,-3.63535768621217,-4.66885193893426));
#29920=CARTESIAN_POINT('Ctrl Pts',(-6.31305853175531,-4.41321055856602,
-4.06318410983209));
#29921=CARTESIAN_POINT('Ctrl Pts',(-6.35947807978292,-5.03641328040699,
-3.25890070630738));
#29922=CARTESIAN_POINT('Ctrl Pts',(-6.40589762781053,-5.42867704267341,
-2.35445736863992));
#29923=CARTESIAN_POINT('Ctrl Pts',(-6.44389002113873,-5.74972797439643,
-1.61420959614342));
#29924=CARTESIAN_POINT('Ctrl Pts',(-6.48188241446693,-5.91607948259785,
-0.806867539943621));
#29925=CARTESIAN_POINT('Ctrl Pts',(-6.51987480779513,-5.91690427471314,
0.000144985681112611));
#29926=CARTESIAN_POINT('Ctrl Pts',(-6.77162519220487,-5.916739287675,0.000155466350801038));
#29927=CARTESIAN_POINT('Ctrl Pts',(-6.73607187764382,-5.91595985127682,
-0.755108201434952));
#29928=CARTESIAN_POINT('Ctrl Pts',(-6.70051856308277,-5.77079135495242,
-1.51066285089507));
#29929=CARTESIAN_POINT('Ctrl Pts',(-6.66496524852172,-5.48865227932844,
-2.21104047700275));
#29930=CARTESIAN_POINT('Ctrl Pts',(-6.61854570049411,-5.12028245128035,
-3.12547597349477));
#29931=CARTESIAN_POINT('Ctrl Pts',(-6.5721261524665,-4.51842228352505,-3.9458525706781));
#29932=CARTESIAN_POINT('Ctrl Pts',(-6.52570660443889,-3.75674795527445,
-4.57174459422911));
#29933=CARTESIAN_POINT('Ctrl Pts',(-6.47928705641128,-2.9950736270239,-5.19763661778009));
#29934=CARTESIAN_POINT('Ctrl Pts',(-6.43286750838367,-2.07358513827807,
-5.62904406769878));
#29935=CARTESIAN_POINT('Ctrl Pts',(-6.38644796035606,-1.10508568598514,
-5.813156583213));
#29936=CARTESIAN_POINT('Ctrl Pts',(-6.34002841232845,-0.13658623369216,
-5.99726909872722));
#29937=CARTESIAN_POINT('Ctrl Pts',(-6.29360886430083,0.878924182148105,
-5.93408667983692));
#29938=CARTESIAN_POINT('Ctrl Pts',(-6.24718931627322,1.8171327536815,-5.63134374637349));
#29939=CARTESIAN_POINT('Ctrl Pts',(-6.2007697682456,2.75534132521499,-5.32860081291002));
#29940=CARTESIAN_POINT('Ctrl Pts',(-6.15435022021799,3.61624805244166,-4.78629736487347));
#29941=CARTESIAN_POINT('Ctrl Pts',(-6.10793067219037,4.29446580107692,-4.0708189983961));
#29942=CARTESIAN_POINT('Ctrl Pts',(-6.06151112416276,4.97268354971214,-3.35534063191877));
#29943=CARTESIAN_POINT('Ctrl Pts',(-6.01509157613515,5.46821231975582,-2.46668734700071));
#29944=CARTESIAN_POINT('Ctrl Pts',(-5.96867202810754,5.72039239584158,-1.51364284820421));
#29945=CARTESIAN_POINT('Ctrl Pts',(-5.92225248007992,5.97257247192732,-0.560598349407762));
#29946=CARTESIAN_POINT('Ctrl Pts',(-5.87583293205231,5.98140385405515,0.456837363267123));
#29947=CARTESIAN_POINT('Ctrl Pts',(-5.8294133840247,5.74580545640615,1.41411579846036));
#29948=CARTESIAN_POINT('Ctrl Pts',(-5.78299383599708,5.51020705875715,2.37139423365359));
#29949=CARTESIAN_POINT('Ctrl Pts',(-5.73657428796947,5.03017888133132,3.26851539136518));
#29950=CARTESIAN_POINT('Ctrl Pts',(-5.69015473994186,4.36448314818263,3.99565897988701));
#29951=CARTESIAN_POINT('Ctrl Pts',(-5.64373519191425,3.6987874150339,4.72280256840889));
#29952=CARTESIAN_POINT('Ctrl Pts',(-5.59731564388664,2.84742412616229,5.27996858774099));
#29953=CARTESIAN_POINT('Ctrl Pts',(-5.55089609585902,1.9146121643015,5.59895205325341));
#29954=CARTESIAN_POINT('Ctrl Pts',(-5.50447654783141,0.981800202440707,
5.91793551876582));
#29955=CARTESIAN_POINT('Ctrl Pts',(-5.45805699980379,-0.0324604324092743,
5.99873643045854));
#29956=CARTESIAN_POINT('Ctrl Pts',(-5.41163745177617,-1.00400992322729,
5.83146361631306));
#29957=CARTESIAN_POINT('Ctrl Pts',(-5.36521790374857,-1.97555941404519,
5.66419080216759));
#29958=CARTESIAN_POINT('Ctrl Pts',(-5.31879835572096,-2.90439776083114,
5.24884426218397));
#29959=CARTESIAN_POINT('Ctrl Pts',(-5.27237880769335,-3.67682204027665,
4.636268275074));
#29960=CARTESIAN_POINT('Ctrl Pts',(-5.22595925966574,-4.44924631972226,
4.02369228796397));
#29961=CARTESIAN_POINT('Ctrl Pts',(-5.17953971163812,-5.06525653182739,
3.21388685372754));
#29962=CARTESIAN_POINT('Ctrl Pts',(-5.13312016361051,-5.44944433223741,
2.30598358714182));
#29963=CARTESIAN_POINT('Ctrl Pts',(-5.09595517314197,-5.75703750250859,
1.57908688773953));
#29964=CARTESIAN_POINT('Ctrl Pts',(-5.05879018267342,-5.91602969878726,
0.78930828952916));
#29965=CARTESIAN_POINT('Ctrl Pts',(-5.02162519220488,-5.91684860187072,
-0.000150428407648674));
#29966=CARTESIAN_POINT('Origin',(-29.75,0.,0.));
#29967=CARTESIAN_POINT('',(-3.01987480779514,-5.9165030994658,0.000139679809713911));
#29968=CARTESIAN_POINT('',(-3.27162519220487,-5.91637946298814,0.000111165658334626));
#29969=CARTESIAN_POINT('',(-29.75,-5.91675,-7.2459289488551E-16));
#29970=CARTESIAN_POINT('Ctrl Pts',(-3.01987480779514,-5.9165030994658,0.000139679809713911));
#29971=CARTESIAN_POINT('Ctrl Pts',(-3.03447992847091,-5.91677227233095,
0.310433725540576));
#29972=CARTESIAN_POINT('Ctrl Pts',(-3.04908504914667,-5.89278908313743,
0.620686564004424));
#29973=CARTESIAN_POINT('Ctrl Pts',(-3.06369016982243,-5.84419449252714,
0.927035418652865));
#29974=CARTESIAN_POINT('Ctrl Pts',(-3.11010971785004,-5.68974599581187,
1.90070593375919));
#29975=CARTESIAN_POINT('Ctrl Pts',(-3.15652926587766,-5.28668219474421,
2.83493984352893));
#29976=CARTESIAN_POINT('Ctrl Pts',(-3.20294881390527,-4.68434378731049,
3.61537373131302));
#29977=CARTESIAN_POINT('Ctrl Pts',(-3.24936836193289,-4.08200537987681,
4.39580761909706));
#29978=CARTESIAN_POINT('Ctrl Pts',(-3.29578790996049,-3.28039236607707,
5.02244148489549));
#29979=CARTESIAN_POINT('Ctrl Pts',(-3.3422074579881,-2.3776334928619,5.41856649934147));
#29980=CARTESIAN_POINT('Ctrl Pts',(-3.38862700601571,-1.47487461964673,
5.81469151378745));
#29981=CARTESIAN_POINT('Ctrl Pts',(-3.43504655404332,-0.4709698870161,5.98030767688098));
#29982=CARTESIAN_POINT('Ctrl Pts',(-3.48146610207094,0.511188596636436,
5.89514123267316));
#29983=CARTESIAN_POINT('Ctrl Pts',(-3.52788565009856,1.49334708028909,5.80997478846532));
#29984=CARTESIAN_POINT('Ctrl Pts',(-3.57430519812617,2.45375931496351,5.47402573695612));
#29985=CARTESIAN_POINT('Ctrl Pts',(-3.62072474615379,3.27485728782222,4.92841898368611));
#29986=CARTESIAN_POINT('Ctrl Pts',(-3.6671442941814,4.09595526068089,4.38281223041613));
#29987=CARTESIAN_POINT('Ctrl Pts',(-3.71356384220902,4.77773897172381,3.62754777538526));
#29988=CARTESIAN_POINT('Ctrl Pts',(-3.75998339023663,5.23674847200481,2.75508064770333));
#29989=CARTESIAN_POINT('Ctrl Pts',(-3.80640293826424,5.69575797228578,1.88261352002145));
#29990=CARTESIAN_POINT('Ctrl Pts',(-3.85282248629185,5.93199326180497,0.892943719688536));
#29991=CARTESIAN_POINT('Ctrl Pts',(-3.89924203431946,5.91653580688652,-0.0927792014856135));
#29992=CARTESIAN_POINT('Ctrl Pts',(-3.94566158234707,5.90107835196807,-1.07850212265976));
#29993=CARTESIAN_POINT('Ctrl Pts',(-3.99208113037469,5.63392815261194,-2.06027816467504));
#29994=CARTESIAN_POINT('Ctrl Pts',(-4.0385006784023,5.14778816379024,-2.91792408316712));
#29995=CARTESIAN_POINT('Ctrl Pts',(-4.08492022642991,4.66164817496857,-3.77557000165915));
#29996=CARTESIAN_POINT('Ctrl Pts',(-4.13133977445751,3.95651839668135,-4.50908579662804));
#29997=CARTESIAN_POINT('Ctrl Pts',(-4.17775932248512,3.11871666601992,-5.02867878189548));
#29998=CARTESIAN_POINT('Ctrl Pts',(-4.22417887051273,2.2809149353584,-5.54827176716297));
#29999=CARTESIAN_POINT('Ctrl Pts',(-4.27059841854035,1.31044125232261,-5.85394194272899));
#30000=CARTESIAN_POINT('Ctrl Pts',(-4.31701796656796,0.326095293021471,
-5.90827096486437));
#30001=CARTESIAN_POINT('Ctrl Pts',(-4.36343751459558,-0.658250666279667,
-5.96259998699975));
#30002=CARTESIAN_POINT('Ctrl Pts',(-4.40985706262319,-1.65646890184619,
-5.76558785570449));
#30003=CARTESIAN_POINT('Ctrl Pts',(-4.45627661065081,-2.54636341275257,
-5.34135163648564));
#30004=CARTESIAN_POINT('Ctrl Pts',(-4.50269615867842,-3.4362579236589,-4.91711541726682));
#30005=CARTESIAN_POINT('Ctrl Pts',(-4.54911570670603,-4.21782870990514,
-4.2656551101244));
#30006=CARTESIAN_POINT('Ctrl Pts',(-4.59553525473364,-4.79540047613297,
-3.46671865139005));
#30007=CARTESIAN_POINT('Ctrl Pts',(-4.64195480276126,-5.37297224236086,
-2.66778219265561));
#30008=CARTESIAN_POINT('Ctrl Pts',(-4.68837435078887,-5.74654498857032,
-1.72136958232917));
#30009=CARTESIAN_POINT('Ctrl Pts',(-4.73479389881649,-5.87038813800455,
-0.743335081620309));
#30010=CARTESIAN_POINT('Ctrl Pts',(-4.7464875351427,-5.90158570050807,-0.496956556801938));
#30011=CARTESIAN_POINT('Ctrl Pts',(-4.75818117146892,-5.9169355219347,-0.248571319372749));
#30012=CARTESIAN_POINT('Ctrl Pts',(-4.76987480779513,-5.91668395451438,
-0.000155206356347026));
#30013=CARTESIAN_POINT('Ctrl Pts',(-5.02162519220488,-5.91684860187072,
-0.000150428407648674));
#30014=CARTESIAN_POINT('Ctrl Pts',(-5.01237063464581,-5.91705251920329,
-0.196735737687811));
#30015=CARTESIAN_POINT('Ctrl Pts',(-5.00311607708674,-5.90744852755087,
-0.393301212035374));
#30016=CARTESIAN_POINT('Ctrl Pts',(-4.99386151952768,-5.88788882431215,
-0.588870976413262));
#30017=CARTESIAN_POINT('Ctrl Pts',(-4.94744197150006,-5.78978012726201,
-1.56982117444776));
#30018=CARTESIAN_POINT('Ctrl Pts',(-4.90102242347245,-5.44119734444683,
-2.5257204715818));
#30019=CARTESIAN_POINT('Ctrl Pts',(-4.85460287544484,-4.88481192839464,
-3.33955330224496));
#30020=CARTESIAN_POINT('Ctrl Pts',(-4.80818332741722,-4.32842651234242,
-4.15338613290818));
#30021=CARTESIAN_POINT('Ctrl Pts',(-4.76176377938962,-3.56423846305318,
-4.82515249710048));
#30022=CARTESIAN_POINT('Ctrl Pts',(-4.715344231362,-2.68579518354086,-5.27261871050719));
#30023=CARTESIAN_POINT('Ctrl Pts',(-4.66892468333439,-1.80735190402854,
-5.72008492391391));
#30024=CARTESIAN_POINT('Ctrl Pts',(-4.62250513530677,-0.814653394293164,
-5.94325098653501));
#30025=CARTESIAN_POINT('Ctrl Pts',(-4.57608558727915,0.170780037086872,
-5.91479822253088));
#30026=CARTESIAN_POINT('Ctrl Pts',(-4.52966603925154,1.1562134684668,-5.88634545852675));
#30027=CARTESIAN_POINT('Ctrl Pts',(-4.48324649122394,2.13438182149134,-5.60627386789744));
#30028=CARTESIAN_POINT('Ctrl Pts',(-4.43682694319633,2.98554348384278,-5.1088681662777));
#30029=CARTESIAN_POINT('Ctrl Pts',(-4.39040739516872,3.83670514619431,-4.61146246465791));
#30030=CARTESIAN_POINT('Ctrl Pts',(-4.3439878471411,4.56086011787267,-3.89672265204767));
#30031=CARTESIAN_POINT('Ctrl Pts',(-4.29756829911349,5.06936160959196,-3.05214296937695));
#30032=CARTESIAN_POINT('Ctrl Pts',(-4.25114875108587,5.57786310131125,-2.20756328670622));
#30033=CARTESIAN_POINT('Ctrl Pts',(-4.20472920305825,5.87071111307149,-1.23314373397488));
#30034=CARTESIAN_POINT('Ctrl Pts',(-4.15830965503064,5.9120569149645,-0.248167017434493));
#30035=CARTESIAN_POINT('Ctrl Pts',(-4.11189010700303,5.9534027168575,0.736809699105835));
#30036=CARTESIAN_POINT('Ctrl Pts',(-4.06547055897542,5.74324630888342,1.73234357945519));
#30037=CARTESIAN_POINT('Ctrl Pts',(-4.01905101094781,5.30731380153418,2.61656722565398));
#30038=CARTESIAN_POINT('Ctrl Pts',(-3.9726314629202,4.87138129418494,3.50079087185276));
#30039=CARTESIAN_POINT('Ctrl Pts',(-3.92621191489259,4.20967268746058,4.27370428390081));
#30040=CARTESIAN_POINT('Ctrl Pts',(-3.87979236686498,3.40319045420619,4.84069195123201));
#30041=CARTESIAN_POINT('Ctrl Pts',(-3.83337281883736,2.59670822095181,5.40767961856321));
#30042=CARTESIAN_POINT('Ctrl Pts',(-3.78695327080975,1.64545236116725,5.7687415411776));
#30043=CARTESIAN_POINT('Ctrl Pts',(-3.74053372278213,0.66587001815382,5.87967864370526));
#30044=CARTESIAN_POINT('Ctrl Pts',(-3.69411417475452,-0.31371232485961,
5.99061574623291));
#30045=CARTESIAN_POINT('Ctrl Pts',(-3.64769462672691,-1.32162115110204,
5.8514280286739));
#30046=CARTESIAN_POINT('Ctrl Pts',(-3.6012750786993,-2.23447419457524,5.47915403215709));
#30047=CARTESIAN_POINT('Ctrl Pts',(-3.55485553067169,-3.14732723804844,
5.10688003564028));
#30048=CARTESIAN_POINT('Ctrl Pts',(-3.50843598264408,-3.96512449875239,
4.50151976016569));
#30049=CARTESIAN_POINT('Ctrl Pts',(-3.46201643461646,-4.58775604955412,
3.73717784753347));
#30050=CARTESIAN_POINT('Ctrl Pts',(-3.41559688658885,-5.21038760035589,
2.97283593490122));
#30051=CARTESIAN_POINT('Ctrl Pts',(-3.36917733856124,-5.6378534412554,2.04951238511135));
#30052=CARTESIAN_POINT('Ctrl Pts',(-3.32275779053362,-5.81782572005508,
1.08023503247858));
#30053=CARTESIAN_POINT('Ctrl Pts',(-3.3057135910907,-5.88390743658177,0.724338492858101));
#30054=CARTESIAN_POINT('Ctrl Pts',(-3.28866939164779,-5.91662229564017,
0.36224650323652));
#30055=CARTESIAN_POINT('Ctrl Pts',(-3.27162519220487,-5.91637946298814,
0.000111165658334626));
#30056=CARTESIAN_POINT('Origin',(-29.75,0.,0.));
#30057=CARTESIAN_POINT('',(-1.26987480779516,-5.91708582682028,-0.000110601437552926));
#30058=CARTESIAN_POINT('',(-1.52162519220488,-5.91720137462112,-6.73836950611244E-5));
#30059=CARTESIAN_POINT('',(-29.75,-5.91675,-7.2459289488551E-16));
#30060=CARTESIAN_POINT('Ctrl Pts',(-1.26987480779516,-5.91708582682028,
-0.000110601437552926));
#30061=CARTESIAN_POINT('Ctrl Pts',(-1.3107786854729,-5.91633930945087,0.868669186826611));
#30062=CARTESIAN_POINT('Ctrl Pts',(-1.35168256315065,-5.72265720390265,
1.73777006268092));
#30063=CARTESIAN_POINT('Ctrl Pts',(-1.39258644082839,-5.35218380498871,
2.52351549592291));
#30064=CARTESIAN_POINT('Ctrl Pts',(-1.439005988856,-4.93175403866376,3.41521452170255));
#30065=CARTESIAN_POINT('Ctrl Pts',(-1.4854255368836,-4.28363963608922,4.19956236932577));
#30066=CARTESIAN_POINT('Ctrl Pts',(-1.53184508491121,-3.48717857307409,
4.78054294561178));
#30067=CARTESIAN_POINT('Ctrl Pts',(-1.57826463293882,-2.69071751005887,
5.36152352189784));
#30068=CARTESIAN_POINT('Ctrl Pts',(-1.62468418096643,-1.74590978660303,
5.73913682684664));
#30069=CARTESIAN_POINT('Ctrl Pts',(-1.67110372899405,-0.768413395098483,
5.86715809605289));
#30070=CARTESIAN_POINT('Ctrl Pts',(-1.71752327702166,0.209082996406062,
5.99517936525915));
#30071=CARTESIAN_POINT('Ctrl Pts',(-1.76394282504928,1.2192680559593,5.87360859872287));
#30072=CARTESIAN_POINT('Ctrl Pts',(-1.8103623730769,2.13848097288002,5.51732755179846));
#30073=CARTESIAN_POINT('Ctrl Pts',(-1.85678192110451,3.05769388980073,5.16104650487406));
#30074=CARTESIAN_POINT('Ctrl Pts',(-1.90320146913213,3.88593466408892,4.57005517756153));
#30075=CARTESIAN_POINT('Ctrl Pts',(-1.94962101715974,4.52181488471369,3.81669936354943));
#30076=CARTESIAN_POINT('Ctrl Pts',(-1.99604056518734,5.15769510533839,3.06334354953742));
#30077=CARTESIAN_POINT('Ctrl Pts',(-2.04246011321495,5.60121477229972,2.14762324882588));
#30078=CARTESIAN_POINT('Ctrl Pts',(-2.08887966124256,5.79808084435675,1.1816354923312));
#30079=CARTESIAN_POINT('Ctrl Pts',(-2.13529920927017,5.99494691641379,0.215647735836411));
#30080=CARTESIAN_POINT('Ctrl Pts',(-2.18171875729779,5.94515939356647,-0.800607476441526));
#30081=CARTESIAN_POINT('Ctrl Pts',(-2.22813830532541,5.65481295806546,-1.74272613311839));
#30082=CARTESIAN_POINT('Ctrl Pts',(-2.27455785335302,5.36446652256445,-2.68484478979524));
#30083=CARTESIAN_POINT('Ctrl Pts',(-2.32097740138064,4.83356117440976,-3.55282689087102));
#30084=CARTESIAN_POINT('Ctrl Pts',(-2.36739694940825,4.12708722822561,-4.2404191917822));
#30085=CARTESIAN_POINT('Ctrl Pts',(-2.41381649743586,3.42061328204151,-4.92801149269334));
#30086=CARTESIAN_POINT('Ctrl Pts',(-2.46023604546347,2.53857073782799,-5.43521399343989));
#30087=CARTESIAN_POINT('Ctrl Pts',(-2.50665559349108,1.58893404870036,-5.69993794139027));
#30088=CARTESIAN_POINT('Ctrl Pts',(-2.55307514151869,0.639297359572737,
-5.96466188934065));
#30089=CARTESIAN_POINT('Ctrl Pts',(-2.59949468954631,-0.37793347446899,
-5.98690728449486));
#30090=CARTESIAN_POINT('Ctrl Pts',(-2.64591423757392,-1.33823504031722,
-5.76395098054405));
#30091=CARTESIAN_POINT('Ctrl Pts',(-2.69233378560153,-2.29853660616546,
-5.54099467659324));
#30092=CARTESIAN_POINT('Ctrl Pts',(-2.73875333362914,-3.2019089038202,-5.07283667353741));
#30093=CARTESIAN_POINT('Ctrl Pts',(-2.78517288165675,-3.93776641472978,
-4.41678611648578));
#30094=CARTESIAN_POINT('Ctrl Pts',(-2.83159242968436,-4.67362392563931,
-3.76073555943419));
#30095=CARTESIAN_POINT('Ctrl Pts',(-2.87801197771197,-5.24196664980369,
-2.91679244838682));
#30096=CARTESIAN_POINT('Ctrl Pts',(-2.92443152573957,-5.57322141570446,
-1.98826733264174));
#30097=CARTESIAN_POINT('Ctrl Pts',(-2.95624595309143,-5.80025250783052,
-1.35188684005969));
#30098=CARTESIAN_POINT('Ctrl Pts',(-2.98806038044329,-5.91591675849993,
-0.675775815500215));
#30099=CARTESIAN_POINT('Ctrl Pts',(-3.01987480779514,-5.9165030994658,0.000139679809713911));
#30100=CARTESIAN_POINT('Ctrl Pts',(-3.27162519220487,-5.91637946298814,
0.000111165658334626));
#30101=CARTESIAN_POINT('Ctrl Pts',(-3.24224984362017,-5.91596094560191,
-0.624022095151271));
#30102=CARTESIAN_POINT('Ctrl Pts',(-3.21287449503547,-5.81764537263417,
-1.24828411611053));
#30103=CARTESIAN_POINT('Ctrl Pts',(-3.18349914645077,-5.62352742823134,
-1.84117981149419));
#30104=CARTESIAN_POINT('Ctrl Pts',(-3.13707959842316,-5.31677814090809,
-2.77808614735848));
#30105=CARTESIAN_POINT('Ctrl Pts',(-3.09066005039555,-4.77080084956173,
-3.63666766361148));
#30106=CARTESIAN_POINT('Ctrl Pts',(-3.04424050236794,-4.0524308805934,-4.31182186463013));
#30107=CARTESIAN_POINT('Ctrl Pts',(-2.99782095434033,-3.33406091162508,
-4.98697606564878));
#30108=CARTESIAN_POINT('Ctrl Pts',(-2.95140140631272,-2.44329826503476,
-5.4787029514331));
#30109=CARTESIAN_POINT('Ctrl Pts',(-2.90498185828511,-1.48918486103517,
-5.72680821087003));
#30110=CARTESIAN_POINT('Ctrl Pts',(-2.8585623102575,-0.535071457035527,
-5.97491347030698));
#30111=CARTESIAN_POINT('Ctrl Pts',(-2.81214276222989,0.482392704373251,
-5.97939710339653));
#30112=CARTESIAN_POINT('Ctrl Pts',(-2.76572321420227,1.43865564932456,-5.73971025024428));
#30113=CARTESIAN_POINT('Ctrl Pts',(-2.71930366617466,2.39491859427582,-5.50002339709204));
#30114=CARTESIAN_POINT('Ctrl Pts',(-2.67288411814704,3.2899803227696,-5.01616605769791));
#30115=CARTESIAN_POINT('Ctrl Pts',(-2.62646457011943,4.01427264626211,-4.34736919943388));
#30116=CARTESIAN_POINT('Ctrl Pts',(-2.58004502209182,4.73856496975463,-3.67857234116986));
#30117=CARTESIAN_POINT('Ctrl Pts',(-2.53362547406421,5.29208788824606,-2.82483596403585));
#30118=CARTESIAN_POINT('Ctrl Pts',(-2.4872059260366,5.60708238414337,-1.89066945055927));
#30119=CARTESIAN_POINT('Ctrl Pts',(-2.44078637800898,5.92207688004071,-0.956502937082576));
#30120=CARTESIAN_POINT('Ctrl Pts',(-2.39436682998137,5.99854295334388,0.0580937127365762));
#30121=CARTESIAN_POINT('Ctrl Pts',(-2.34794728195375,5.82712007728882,1.02891954948094));
#30122=CARTESIAN_POINT('Ctrl Pts',(-2.30152773392615,5.65569720123378,1.99974538622514));
#30123=CARTESIAN_POINT('Ctrl Pts',(-2.25510818589853,5.23638537582048,2.92680040989459));
#30124=CARTESIAN_POINT('Ctrl Pts',(-2.20868863787092,4.62051428694949,3.69659999997161));
#30125=CARTESIAN_POINT('Ctrl Pts',(-2.16226908984331,4.00464319807843,4.46639959004873));
#30126=CARTESIAN_POINT('Ctrl Pts',(-2.1158495418157,3.19221284574972,5.07894374653346));
#30127=CARTESIAN_POINT('Ctrl Pts',(-2.06942999378809,2.28267617120534,5.4592484214001));
#30128=CARTESIAN_POINT('Ctrl Pts',(-2.02301044576047,1.37313949666091,5.83955309626675));
#30129=CARTESIAN_POINT('Ctrl Pts',(-1.97659089773286,0.366496499900915,
5.98761828951517));
#30130=CARTESIAN_POINT('Ctrl Pts',(-1.93017134970524,-0.614025507383721,
5.88531872740078));
#30131=CARTESIAN_POINT('Ctrl Pts',(-1.88375180167762,-1.59454751466825,
5.78301916528641));
#30132=CARTESIAN_POINT('Ctrl Pts',(-1.83733225365001,-2.54894853247744,
5.43035484780929));
#30133=CARTESIAN_POINT('Ctrl Pts',(-1.7909127056224,-3.36039640789849,4.87049687332077));
#30134=CARTESIAN_POINT('Ctrl Pts',(-1.74449315759478,-4.17184428331958,
4.31063889883221));
#30135=CARTESIAN_POINT('Ctrl Pts',(-1.69807360956717,-4.84033901635253,
3.54358726733221));
#30136=CARTESIAN_POINT('Ctrl Pts',(-1.65165406153956,-5.28404741237419,
2.66323990838002));
#30137=CARTESIAN_POINT('Ctrl Pts',(-1.60831110509467,-5.69834773411708,
1.84124015058956));
#30138=CARTESIAN_POINT('Ctrl Pts',(-1.56496814864977,-5.91667103198986,
0.920464996667376));
#30139=CARTESIAN_POINT('Ctrl Pts',(-1.52162519220488,-5.91720137462112,
-6.73836950611244E-5));
#30140=CARTESIAN_POINT('Origin',(-62.8183905640093,0.,0.));
#30141=CARTESIAN_POINT('',(-0.69339056400935,-4.91852915329511,-9.19365388711588E-5));
#30142=CARTESIAN_POINT('',(-0.348109435990813,-4.91783243427629,2.96545098249501E-5));
#30143=CARTESIAN_POINT('',(-62.8183905640093,-4.91825,1.40632325245411E-12));
#30144=CARTESIAN_POINT('',(-3.12250225675825E-15,3.9094845766438,-2.98454410297281));
#30145=CARTESIAN_POINT('Ctrl Pts',(-0.69339056400935,-4.91852915329511,
-9.19365388716252E-5));
#30146=CARTESIAN_POINT('Ctrl Pts',(-0.687874893659468,-4.91861282933523,
-0.0974721923576648));
#30147=CARTESIAN_POINT('Ctrl Pts',(-0.635939675281974,-4.89194258344,-1.01435309429727));
#30148=CARTESIAN_POINT('Ctrl Pts',(-0.537584908876869,-4.34627971767338,
-2.721289900206));
#30149=CARTESIAN_POINT('Ctrl Pts',(-0.398326264794041,-2.50959877852527,
-4.47185006834336));
#30150=CARTESIAN_POINT('Ctrl Pts',(-0.259067620711191,-0.0584880437401866,
-5.12759583452146));
#30151=CARTESIAN_POINT('Ctrl Pts',(-0.12629219911318,2.29214640132989,-4.55583897742123));
#30152=CARTESIAN_POINT('Ctrl Pts',(-0.0399363255427856,3.48109416590671,
-3.54459219221265));
#30153=CARTESIAN_POINT('Ctrl Pts',(-3.25477492180148E-15,3.9094845766438,
-2.98454410297281));
#30154=CARTESIAN_POINT('',(0.,-1.55153804394499,-4.66710967952236));
#30155=CARTESIAN_POINT('Origin',(0.,0.,0.));
#30156=CARTESIAN_POINT('Ctrl Pts',(-0.348109435990813,-4.91783243427629,
2.96545098246725E-5));
#30157=CARTESIAN_POINT('Ctrl Pts',(-0.324912053382433,-4.91783717729381,
-0.409677115258361));
#30158=CARTESIAN_POINT('Ctrl Pts',(-0.255295122746436,-4.76590055786429,
-1.63925672502214));
#30159=CARTESIAN_POINT('Ctrl Pts',(-0.139258644082833,-3.75247085555401,
-3.49516562013044));
#30160=CARTESIAN_POINT('Ctrl Pts',(-0.0464195480276115,-2.32937887075175,
-4.40852359138744));
#30161=CARTESIAN_POINT('Ctrl Pts',(0.,-1.55153804394499,-4.66710967952236));
#30162=CARTESIAN_POINT('Origin',(-62.8183905640093,0.,0.));
#30163=CARTESIAN_POINT('',(-2.44339056400933,-4.91804476595219,0.000116107698993155));
#30164=CARTESIAN_POINT('',(-2.0981094359908,-4.91862520145862,-5.60121431075755E-5));
#30165=CARTESIAN_POINT('',(-62.8183905640093,-4.91825,1.40632325245411E-12));
#30166=CARTESIAN_POINT('Ctrl Pts',(-2.44339056400934,-4.9180447659522,0.000116107698993062));
#30167=CARTESIAN_POINT('Ctrl Pts',(-2.41157613665747,-4.91755737482448,
-0.561733114392291));
#30168=CARTESIAN_POINT('Ctrl Pts',(-2.333342161278,-4.68112996827926,-1.94376062201184));
#30169=CARTESIAN_POINT('Ctrl Pts',(-2.20868863787092,-3.41248139082355,
-3.82760144861539));
#30170=CARTESIAN_POINT('Ctrl Pts',(-2.06942999378809,-1.15971890993101,
-4.99505897100328));
#30171=CARTESIAN_POINT('Ctrl Pts',(-1.93017134970524,1.37697549976642,-4.93958506317368));
#30172=CARTESIAN_POINT('Ctrl Pts',(-1.79091270562242,3.57654743186344,-3.67476128358358));
#30173=CARTESIAN_POINT('Ctrl Pts',(-1.65165406153958,4.90047960504737,-1.51025223624387));
#30174=CARTESIAN_POINT('Ctrl Pts',(-1.51239541745672,5.02463601739066,1.02400924064084));
#30175=CARTESIAN_POINT('Ctrl Pts',(-1.3731367733739,3.91861974053298,3.3075642508956));
#30176=CARTESIAN_POINT('Ctrl Pts',(-1.23387812929106,1.85321465084221,4.7813343589219));
#30177=CARTESIAN_POINT('Ctrl Pts',(-1.09461948520821,-0.665909531765221,
5.08449847225302));
#30178=CARTESIAN_POINT('Ctrl Pts',(-0.955360841125384,-3.0220005881154,
4.1428345670361));
#30179=CARTESIAN_POINT('Ctrl Pts',(-0.821617867392433,-4.57420574358984,
2.26435637255426));
#30180=CARTESIAN_POINT('Ctrl Pts',(-0.734294441687084,-4.91790861684306,
0.722074150186002));
#30181=CARTESIAN_POINT('Ctrl Pts',(-0.69339056400935,-4.91852915329511,
-9.19365388716252E-5));
#30182=CARTESIAN_POINT('Ctrl Pts',(-2.0981094359908,-4.91862520145862,-5.60121431077924E-5));
#30183=CARTESIAN_POINT('Ctrl Pts',(-2.09503284440806,-4.9186564935966,-0.054370759900058));
#30184=CARTESIAN_POINT('Ctrl Pts',(-2.0455367047977,-4.90448501505777,-0.928168902546578));
#30185=CARTESIAN_POINT('Ctrl Pts',(-1.94962101715972,-4.41626575409672,
-2.60617701967216));
#30186=CARTESIAN_POINT('Ctrl Pts',(-1.8103623730769,-2.62620047284534,-4.40438801630634));
#30187=CARTESIAN_POINT('Ctrl Pts',(-1.67110372899405,-0.193167284512309,
-5.12428009940892));
#30188=CARTESIAN_POINT('Ctrl Pts',(-1.53184508491121,2.28715890535059,-4.58960454528829));
#30189=CARTESIAN_POINT('Ctrl Pts',(-1.39258644082838,4.20752364775137,-2.93126272184108));
#30190=CARTESIAN_POINT('Ctrl Pts',(-1.25332779674554,5.0977685824936,-0.555268006901366));
#30191=CARTESIAN_POINT('Ctrl Pts',(-1.1140691526627,4.73993440187225,1.95667777727522));
#30192=CARTESIAN_POINT('Ctrl Pts',(-0.974810508579856,3.22163334032844,
3.98956232001804));
#30193=CARTESIAN_POINT('Ctrl Pts',(-0.835551864497027,0.914579917925479,
5.04571140862161));
#30194=CARTESIAN_POINT('Ctrl Pts',(-0.696293220414185,-1.61637760332782,
4.86648495952254));
#30195=CARTESIAN_POINT('Ctrl Pts',(-0.55703457633135,-3.75162148741517,
3.49588943240163));
#30196=CARTESIAN_POINT('Ctrl Pts',(-0.440973314856899,-4.7656461069887,
1.64014823529778));
#30197=CARTESIAN_POINT('Ctrl Pts',(-0.371331601410049,-4.91782768619158,
0.410174132512313));
#30198=CARTESIAN_POINT('Ctrl Pts',(-0.348109435990813,-4.91783243427629,
2.96545098246725E-5));
#30199=CARTESIAN_POINT('Origin',(-62.8183905640093,0.,0.));
#30200=CARTESIAN_POINT('',(-4.19339056400932,-4.91819510023076,-0.000129014012458647));
#30201=CARTESIAN_POINT('',(-3.84810943599078,-4.91794199414229,9.24055450682304E-5));
#30202=CARTESIAN_POINT('',(-62.8183905640093,-4.91825,1.40632325245411E-12));
#30203=CARTESIAN_POINT('Ctrl Pts',(-4.19339056400932,-4.91819510023076,
-0.000129014012458656));
#30204=CARTESIAN_POINT('Ctrl Pts',(-4.1816969276831,-4.91840421358947,-0.206622874297924));
#30205=CARTESIAN_POINT('Ctrl Pts',(-4.12358374332926,-4.85499449889969,
-1.23269585591806));
#30206=CARTESIAN_POINT('Ctrl Pts',(-4.01905101094782,-4.15570990356999,
-3.0042698423568));
#30207=CARTESIAN_POINT('Ctrl Pts',(-3.87979236686497,-2.20668695036655,
-4.62883298374532));
#30208=CARTESIAN_POINT('Ctrl Pts',(-3.74053372278213,0.28259525882338,-5.12012714764091));
#30209=CARTESIAN_POINT('Ctrl Pts',(-3.60127507869929,2.70269017153252,-4.35786965443408));
#30210=CARTESIAN_POINT('Ctrl Pts',(-3.46201643461646,4.46109023849236,-2.52868265552132));
#30211=CARTESIAN_POINT('Ctrl Pts',(-3.32275779053363,5.12728948705797,-0.0804027626875136));
#30212=CARTESIAN_POINT('Ctrl Pts',(-3.18349914645079,4.53818353564321,2.38756199608455));
#30213=CARTESIAN_POINT('Ctrl Pts',(-3.04424050236796,2.83800215050638,4.27098418189009));
#30214=CARTESIAN_POINT('Ctrl Pts',(-2.90498185828511,0.442997727543895,
5.10874887834615));
#30215=CARTESIAN_POINT('Ctrl Pts',(-2.76572321420227,-2.06046504404221,
4.69574763908411));
#30216=CARTESIAN_POINT('Ctrl Pts',(-2.62646457011944,-4.05946780997995,
3.13309482607209));
#30217=CARTESIAN_POINT('Ctrl Pts',(-2.51902035338846,-4.83497050962448,
1.33561036528277));
#30218=CARTESIAN_POINT('Ctrl Pts',(-2.45799568468509,-4.91826851369274,
0.258045492989058));
#30219=CARTESIAN_POINT('Ctrl Pts',(-2.44339056400934,-4.9180447659522,0.000116107698993062));
#30220=CARTESIAN_POINT('Ctrl Pts',(-3.84810943599078,-4.91794199414229,
9.24055450680916E-5));
#30221=CARTESIAN_POINT('Ctrl Pts',(-3.81873408740606,-4.91759410499135,
-0.518713258033689));
#30222=CARTESIAN_POINT('Ctrl Pts',(-3.74293919079372,-4.70672807007167,
-1.85762278311962));
#30223=CARTESIAN_POINT('Ctrl Pts',(-3.62072474615378,-3.51184999623001,
-3.73663908038491));
#30224=CARTESIAN_POINT('Ctrl Pts',(-3.48146610207094,-1.29053252299245,
-4.96287092523671));
#30225=CARTESIAN_POINT('Ctrl Pts',(-3.3422074579881,1.24674374109644,-4.97405187513803));
#30226=CARTESIAN_POINT('Ctrl Pts',(-3.20294881390526,3.47878194424713,-3.76744451832491));
#30227=CARTESIAN_POINT('Ctrl Pts',(-3.06369016982243,4.8591161279818,-1.63846039519689));
#30228=CARTESIAN_POINT('Ctrl Pts',(-2.92443152573959,5.04980152031218,0.891665082289887));
#30229=CARTESIAN_POINT('Ctrl Pts',(-2.78517288165675,4.0041529537823,3.20348577954525));
#30230=CARTESIAN_POINT('Ctrl Pts',(-2.64591423757392,1.9781747155564,4.73100272599303));
#30231=CARTESIAN_POINT('Ctrl Pts',(-2.50665559349108,-0.532116534951586,
5.10023666524732));
#30232=CARTESIAN_POINT('Ctrl Pts',(-2.36739694940823,-2.91213063348896,
4.22078868480285));
#30233=CARTESIAN_POINT('Ctrl Pts',(-2.23121489690814,-4.54234358429553,
2.35023168290226));
#30234=CARTESIAN_POINT('Ctrl Pts',(-2.14145239243567,-4.91818435848776,
0.76512899309031));
#30235=CARTESIAN_POINT('Ctrl Pts',(-2.0981094359908,-4.91862520145862,-5.60121431077924E-5));
#30236=CARTESIAN_POINT('Origin',(-62.8183905640093,0.,0.));
#30237=CARTESIAN_POINT('',(-5.94339056400932,-4.91837823959233,0.000120518161154786));
#30238=CARTESIAN_POINT('',(-5.59810943599078,-4.91833196199783,-0.000125042380879348));
#30239=CARTESIAN_POINT('',(-62.8183905640093,-4.91825,1.40632325245411E-12));
#30240=CARTESIAN_POINT('Ctrl Pts',(-5.94339056400932,-4.91837823959232,
0.000120518161154867));
#30241=CARTESIAN_POINT('Ctrl Pts',(-5.90539817068111,-4.91769263789875,
-0.670702037152937));
#30242=CARTESIAN_POINT('Ctrl Pts',(-5.82098622932529,-4.61046423753281,
-2.16175199008866));
#30243=CARTESIAN_POINT('Ctrl Pts',(-5.69015473994187,-3.150412987362,-4.0460425229334));
#30244=CARTESIAN_POINT('Ctrl Pts',(-5.55089609585902,-0.825006475908536,
-5.06111908603556));
#30245=CARTESIAN_POINT('Ctrl Pts',(-5.41163745177619,1.70238490919671,-4.83709083119842));
#30246=CARTESIAN_POINT('Ctrl Pts',(-5.27237880769335,3.81298441347213,-3.42880619909369));
#30247=CARTESIAN_POINT('Ctrl Pts',(-5.13312016361051,4.99005770009789,-1.18105302083279));
#30248=CARTESIAN_POINT('Ctrl Pts',(-4.99386151952767,4.94542400198837,1.35585527578786));
#30249=CARTESIAN_POINT('Ctrl Pts',(-4.85460287544484,3.69001090836444,3.56081192770356));
#30250=CARTESIAN_POINT('Ctrl Pts',(-4.715344231362,1.53117898244731,4.89398130483108));
#30251=CARTESIAN_POINT('Ctrl Pts',(-4.57608558727916,-1.00252878061676,
5.0289659108369));
#30252=CARTESIAN_POINT('Ctrl Pts',(-4.43682694319632,-3.29078919872254,
3.93271770381442));
#30253=CARTESIAN_POINT('Ctrl Pts',(-4.30926193543972,-4.64887815341735,
2.04653215326229));
#30254=CARTESIAN_POINT('Ctrl Pts',(-4.22811647571071,-4.91757410845133,
0.613083793287724));
#30255=CARTESIAN_POINT('Ctrl Pts',(-4.19339056400932,-4.91819510023076,
-0.000129014012458656));
#30256=CARTESIAN_POINT('Ctrl Pts',(-5.59810943599078,-4.91833196199783,
-0.000125042380879781));
#30257=CARTESIAN_POINT('Ctrl Pts',(-5.58885487843169,-4.9185014666112,-0.163534971373931));
#30258=CARTESIAN_POINT('Ctrl Pts',(-5.53318077284498,-4.87047543051452,
-1.1464867385219));
#30259=CARTESIAN_POINT('Ctrl Pts',(-5.43108711923067,-4.23319416364483,
-2.89406793044928));
#30260=CARTESIAN_POINT('Ctrl Pts',(-5.29182847514784,-2.32751898381641,
-4.56926880289899));
#30261=CARTESIAN_POINT('Ctrl Pts',(-5.15256983106498,0.147998544643936,
-5.12578369071063));
#30262=CARTESIAN_POINT('Ctrl Pts',(-5.01331118698215,2.58728185166053,-4.42736204000073));
#30263=CARTESIAN_POINT('Ctrl Pts',(-4.87405254289932,4.39312552738983,-2.64499718596595));
#30264=CARTESIAN_POINT('Ctrl Pts',(-4.73479389881648,5.12340806451229,-0.215062357612596));
#30265=CARTESIAN_POINT('Ctrl Pts',(-4.59553525473364,4.59933568346607,2.26752580668157));
#30266=CARTESIAN_POINT('Ctrl Pts',(-4.45627661065081,2.94921609668853,4.19495964559934));
#30267=CARTESIAN_POINT('Ctrl Pts',(-4.31701796656797,0.57704515873205,5.09534894761389));
#30268=CARTESIAN_POINT('Ctrl Pts',(-4.17775932248513,-1.93640272295992,
4.74825299533382));
#30269=CARTESIAN_POINT('Ctrl Pts',(-4.03850067840229,-3.97576455713786,
3.2386506757228));
#30270=CARTESIAN_POINT('Ctrl Pts',(-3.92861738290418,-4.81688766647458,
1.42183000652332));
#30271=CARTESIAN_POINT('Ctrl Pts',(-3.86515363543367,-4.91814384679624,
0.301114440283927));
#30272=CARTESIAN_POINT('Ctrl Pts',(-3.84810943599078,-4.91794199414229,
9.24055450680916E-5));
#30273=CARTESIAN_POINT('Origin',(-62.8183905640093,0.,0.));
#30274=CARTESIAN_POINT('',(-7.69339056400932,-4.91791353327688,-8.21695429248617E-5));
#30275=CARTESIAN_POINT('',(-7.34810943599077,-4.91824109546754,0.000129230132873345));
#30276=CARTESIAN_POINT('',(-62.8183905640093,-4.91825,1.40632325245411E-12));
#30277=CARTESIAN_POINT('Ctrl Pts',(-7.69339056400932,-4.91791353327688,
-8.21695429247329E-5));
#30278=CARTESIAN_POINT('Ctrl Pts',(-7.67551896170675,-4.91810032602428,
-0.315722413110651));
#30279=CARTESIAN_POINT('Ctrl Pts',(-7.61122781137655,-4.81048024208871,
-1.45107819583804));
#30280=CARTESIAN_POINT('Ctrl Pts',(-7.50051711301875,-3.94674387586246,
-3.27395401108));
#30281=CARTESIAN_POINT('Ctrl Pts',(-7.36125846893591,-1.89400947691462,
-4.7653216249989));
#30282=CARTESIAN_POINT('Ctrl Pts',(-7.22199982485306,0.622431906234182,
-5.09000398923479));
#30283=CARTESIAN_POINT('Ctrl Pts',(-7.08274118077025,2.98648438867875,-4.16850969586284));
#30284=CARTESIAN_POINT('Ctrl Pts',(-6.94348253668739,4.61936119005255,-2.22644655991574));
#30285=CARTESIAN_POINT('Ctrl Pts',(-6.80422389260458,5.12128797640124,0.260713542211845));
#30286=CARTESIAN_POINT('Ctrl Pts',(-6.66496524852172,4.36937890199675,2.68404360976314));
#30287=CARTESIAN_POINT('Ctrl Pts',(-6.52570660443889,2.54772253320329,4.45024403624483));
#30288=CARTESIAN_POINT('Ctrl Pts',(-6.38644796035604,0.102311770964511,
5.12689910080611));
#30289=CARTESIAN_POINT('Ctrl Pts',(-6.24718931627322,-2.3681478008713,4.54834454296868));
#30290=CARTESIAN_POINT('Ctrl Pts',(-6.10793067219037,-4.25881794278671,
2.85622684997581));
#30291=CARTESIAN_POINT('Ctrl Pts',(-6.00666442143574,-4.87546116306589,
1.11724409472842));
#30292=CARTESIAN_POINT('Ctrl Pts',(-5.95181771870872,-4.91853031402165,
0.14891676273157));
#30293=CARTESIAN_POINT('Ctrl Pts',(-5.94339056400932,-4.91837823959232,
0.000120518161154867));
#30294=CARTESIAN_POINT('Ctrl Pts',(-7.34810943599077,-4.91824109546754,
0.000129230132873172));
#30295=CARTESIAN_POINT('Ctrl Pts',(-7.3125561214297,-4.9175931953426,-0.627677510745102));
#30296=CARTESIAN_POINT('Ctrl Pts',(-7.23058325884101,-4.63937228605784,
-2.07572654968798));
#30297=CARTESIAN_POINT('Ctrl Pts',(-7.10219084822472,-3.25561019578073,
-3.96188897702852));
#30298=CARTESIAN_POINT('Ctrl Pts',(-6.96293220414188,-0.957670908279476,
-5.03770071010642));
#30299=CARTESIAN_POINT('Ctrl Pts',(-6.82367356005904,1.57473325078029,-4.88014110472828));
#30300=CARTESIAN_POINT('Ctrl Pts',(-6.68441491597621,3.72159825835185,-3.52778519989586));
#30301=CARTESIAN_POINT('Ctrl Pts',(-6.54515627189337,4.95731095870299,-1.31172789552367));
#30302=CARTESIAN_POINT('Ctrl Pts',(-6.40589762781053,4.97933400098995,1.22547742523351));
#30303=CARTESIAN_POINT('Ctrl Pts',(-6.26663898372769,3.78227552279275,3.46265127941791));
#30304=CARTESIAN_POINT('Ctrl Pts',(-6.12738033964487,1.65920923023726,4.8520703564012));
#30305=CARTESIAN_POINT('Ctrl Pts',(-5.988121695562,-0.870078318172324,5.05356564550398));
#30306=CARTESIAN_POINT('Ctrl Pts',(-5.84886305147918,-3.18634613365232,
4.01780541212868));
#30307=CARTESIAN_POINT('Ctrl Pts',(-5.71885896495544,-4.62041956406219,
2.13257618342603));
#30308=CARTESIAN_POINT('Ctrl Pts',(-5.6352744264593,-4.91765125551345,0.656106053996394));
#30309=CARTESIAN_POINT('Ctrl Pts',(-5.59810943599078,-4.91833196199783,
-0.000125042380879781));
#30310=CARTESIAN_POINT('Origin',(-62.8183905640093,0.,0.));
#30311=CARTESIAN_POINT('',(-9.44339056400932,-4.91864811437696,4.17001171947731E-5));
#30312=CARTESIAN_POINT('',(-9.09810943599077,-4.91800701852089,-0.000109254779623313));
#30313=CARTESIAN_POINT('',(-62.8183905640093,-4.91825,1.40632325245411E-12));
#30314=CARTESIAN_POINT('Ctrl Pts',(-9.44339056400932,-4.91864811437696,
4.17001171945739E-5));
#30315=CARTESIAN_POINT('Ctrl Pts',(-9.39922020470476,-4.91830005980813,
-0.779739888198681));
#30316=CARTESIAN_POINT('Ctrl Pts',(-9.30863029737259,-4.5312235699483,-2.37934338565543));
#30317=CARTESIAN_POINT('Ctrl Pts',(-9.1716208420128,-2.87439939474084,-4.24657393763936));
#30318=CARTESIAN_POINT('Ctrl Pts',(-9.03236219792996,-0.486642181365819,
-5.1047763394335));
#30319=CARTESIAN_POINT('Ctrl Pts',(-8.89310355384714,2.02025877498237,-4.71318539529599));
#30320=CARTESIAN_POINT('Ctrl Pts',(-8.75384490976428,4.03254335518717,-3.16767362221242));
#30321=CARTESIAN_POINT('Ctrl Pts',(-8.61458626568145,5.05754749108297,-0.846625929064747));
#30322=CARTESIAN_POINT('Ctrl Pts',(-8.47532762159861,4.84432123630313,1.681699690143));
#30323=CARTESIAN_POINT('Ctrl Pts',(-8.33606897751578,3.44506839698563,3.79829775404922));
#30324=CARTESIAN_POINT('Ctrl Pts',(-8.19681033343293,1.20236556641743,4.98496530910879));
#30325=CARTESIAN_POINT('Ctrl Pts',(-8.0575516893501,-1.33471029528195,4.95117264049567));
#30326=CARTESIAN_POINT('Ctrl Pts',(-7.91829304526727,-3.54501140038643,
3.70519314738851));
#30327=CARTESIAN_POINT('Ctrl Pts',(-7.796906003487,-4.7151205220378,1.82839543316926));
#30328=CARTESIAN_POINT('Ctrl Pts',(-7.72193850973436,-4.91761515212871,
0.504118874630245));
#30329=CARTESIAN_POINT('Ctrl Pts',(-7.69339056400932,-4.91791353327688,
-8.21695429247329E-5));
#30330=CARTESIAN_POINT('Ctrl Pts',(-9.09810943599077,-4.91800701852089,
-0.000109254779623522));
#30331=CARTESIAN_POINT('Ctrl Pts',(-9.08267691245533,-4.91822704331746,
-0.272656737973705));
#30332=CARTESIAN_POINT('Ctrl Pts',(-9.02082484089228,-4.82897064533397,
-1.36485826043635));
#30333=CARTESIAN_POINT('Ctrl Pts',(-8.9125532213016,-4.03138450511247,-3.16914830595081));
#30334=CARTESIAN_POINT('Ctrl Pts',(-8.77329457721876,-2.01853479244033,
-4.71392398166109));
#30335=CARTESIAN_POINT('Ctrl Pts',(-8.63403593313593,0.488509216784092,
-5.10459800163426));
#30336=CARTESIAN_POINT('Ctrl Pts',(-8.49477728905309,2.87595238006221,-4.24552233780323));
#30337=CARTESIAN_POINT('Ctrl Pts',(-8.35551864497026,4.5592812180853,-2.34702296273093));
#30338=CARTESIAN_POINT('Ctrl Pts',(-8.21626000088742,5.1263693141631,0.126093885571429));
#30339=CARTESIAN_POINT('Ctrl Pts',(-8.07700135680457,4.43837749456725,2.56833939129752));
#30340=CARTESIAN_POINT('Ctrl Pts',(-7.93774271272176,2.66374557742339,4.38178291474247));
#30341=CARTESIAN_POINT('Ctrl Pts',(-7.7984840686389,0.236953550501235,5.12244229133686));
#30342=CARTESIAN_POINT('Ctrl Pts',(-7.65922542455607,-2.24785139432755,
4.60898319829779));
#30343=CARTESIAN_POINT('Ctrl Pts',(-7.51996678047323,-4.18231886529451,
2.96711491556586));
#30344=CARTESIAN_POINT('Ctrl Pts',(-7.41626145095147,-4.86037762657564,
1.20345049757124));
#30345=CARTESIAN_POINT('Ctrl Pts',(-7.35897566945731,-4.91843911453011,
0.19200710994428));
#30346=CARTESIAN_POINT('Ctrl Pts',(-7.34810943599077,-4.91824109546754,
0.000129230132873172));
#30347=CARTESIAN_POINT('Origin',(-62.8183905640093,0.,0.));
#30348=CARTESIAN_POINT('',(-11.1933905640093,-4.91782725633716,1.39428353682031E-5));
#30349=CARTESIAN_POINT('',(-10.8481094359908,-4.91856570422813,8.11450425239682E-5));
#30350=CARTESIAN_POINT('',(-62.8183905640093,-4.91825,1.40632325245411E-12));
#30351=CARTESIAN_POINT('Ctrl Pts',(-11.1933905640093,-4.91782725633716,
1.3942835367757E-5));
#30352=CARTESIAN_POINT('Ctrl Pts',(-11.1693409957304,-4.91778551848492,
-0.424760092808996));
#30353=CARTESIAN_POINT('Ctrl Pts',(-11.0988718794239,-4.7582004889199,-1.66944734820506));
#30354=CARTESIAN_POINT('Ctrl Pts',(-10.9819832150897,-3.72030772957414,
-3.52914614115021));
#30355=CARTESIAN_POINT('Ctrl Pts',(-10.8427245710069,-1.57294823922665,
-4.88071674296288));
#30356=CARTESIAN_POINT('Ctrl Pts',(-10.703465926924,0.959513381393236,-5.03735011283231));
#30357=CARTESIAN_POINT('Ctrl Pts',(-10.5642072828412,3.25705904102695,-3.96069798035511));
#30358=CARTESIAN_POINT('Ctrl Pts',(-10.4249486387583,4.75718470689197,-1.91435517938488));
#30359=CARTESIAN_POINT('Ctrl Pts',(-10.2856899946755,5.09261727031618,0.60067580807126));
#30360=CARTESIAN_POINT('Ctrl Pts',(-10.1464313505927,4.18123337115581,2.96864440178638));
#30361=CARTESIAN_POINT('Ctrl Pts',(-10.0071727065098,2.24616551454361,4.60980504681049));
#30362=CARTESIAN_POINT('Ctrl Pts',(-9.86791406242699,-0.238827064970182,
5.12235529042668));
#30363=CARTESIAN_POINT('Ctrl Pts',(-9.72865541834415,-2.66534803734968,
4.38080836468806));
#30364=CARTESIAN_POINT('Ctrl Pts',(-9.58939677426131,-4.43931657252653,
2.56671588946183));
#30365=CARTESIAN_POINT('Ctrl Pts',(-9.49430848948303,-4.90847969436099,
0.898935409588413));
#30366=CARTESIAN_POINT('Ctrl Pts',(-9.44563975273237,-4.91866583758374,
0.039748779310035));
#30367=CARTESIAN_POINT('Ctrl Pts',(-9.44339056400932,-4.91864811437696,
4.17001171945739E-5));
#30368=CARTESIAN_POINT('Ctrl Pts',(-10.8481094359908,-4.91856570422813,
8.11450425238988E-5));
#30369=CARTESIAN_POINT('Ctrl Pts',(-10.8063781554533,-4.91799158127243,
-0.736676875350269));
#30370=CARTESIAN_POINT('Ctrl Pts',(-10.7182273268883,-4.5635503776824,-2.29349712765718));
#30371=CARTESIAN_POINT('Ctrl Pts',(-10.5836569502957,-2.98495955491563,
-4.16960171583444));
#30372=CARTESIAN_POINT('Ctrl Pts',(-10.4443983062128,-0.620570198026758,
-5.09023129557908));
#30373=CARTESIAN_POINT('Ctrl Pts',(-10.30513966213,1.89575226084471,-4.76462856670633));
#30374=CARTESIAN_POINT('Ctrl Pts',(-10.1658810180471,3.94794105281364,-3.27251026838425));
#30375=CARTESIAN_POINT('Ctrl Pts',(-10.0266223739643,5.03356243225522,-0.979189079677917));
#30376=CARTESIAN_POINT('Ctrl Pts',(-9.88736372988145,4.88682564047436,1.55386523636191));
#30377=CARTESIAN_POINT('Ctrl Pts',(-9.74810508579864,3.54365598619697,3.7064894799071));
#30378=CARTESIAN_POINT('Ctrl Pts',(-9.6088464417158,1.33289931589153,4.95166047168699));
#30379=CARTESIAN_POINT('Ctrl Pts',(-9.46958779763295,-1.20418873213356,
4.98452520412669));
#30380=CARTESIAN_POINT('Ctrl Pts',(-9.33032915355013,-3.44645738659569,
3.79703746301662));
#30381=CARTESIAN_POINT('Ctrl Pts',(-9.20650303300273,-4.68995778663268,
1.91454404906327));
#30382=CARTESIAN_POINT('Ctrl Pts',(-9.12909646048294,-4.91756522986951,
0.54713990493291));
#30383=CARTESIAN_POINT('Ctrl Pts',(-9.09810943599077,-4.91800701852089,
-0.000109254779623522));
#30384=CARTESIAN_POINT('Origin',(-62.8183905640093,0.,0.));
#30385=CARTESIAN_POINT('',(-12.9433905640093,-4.91859595699376,-6.98021618343542E-5));
#30386=CARTESIAN_POINT('',(-12.5981094359908,-4.9178331468155,-2.64215081000052E-5));
#30387=CARTESIAN_POINT('',(-62.8183905640093,-4.91825,1.40632325245411E-12));
#30388=CARTESIAN_POINT('Ctrl Pts',(-12.9433905640093,-4.91859595699376,
-6.98021618345673E-5));
#30389=CARTESIAN_POINT('Ctrl Pts',(-12.939461786756,-4.91864391970094,-0.0694303996811109));
#30390=CARTESIAN_POINT('Ctrl Pts',(-12.8891134614751,-4.9002331927105,-0.958279418825322));
#30391=CARTESIAN_POINT('Ctrl Pts',(-12.7923455881666,-4.39215783380509,
-2.64660379567266));
#30392=CARTESIAN_POINT('Ctrl Pts',(-12.6530869440837,-2.58566237748044,
-4.42830804687374));
#30393=CARTESIAN_POINT('Ctrl Pts',(-12.5138283000009,-0.146123782862334,
-5.12583748556338));
#30394=CARTESIAN_POINT('Ctrl Pts',(-12.3745696559181,2.3291900385944,-4.56841721523299));
#30395=CARTESIAN_POINT('Ctrl Pts',(-12.2353110118352,4.23425239003886,-2.8925194529639));
#30396=CARTESIAN_POINT('Ctrl Pts',(-12.0960523677524,5.1026502315838,-0.50845127833681));
#30397=CARTESIAN_POINT('Ctrl Pts',(-11.9567937236695,4.72177525841466,2.00010012183084));
#30398=CARTESIAN_POINT('Ctrl Pts',(-11.8175350795867,3.18487641533271,4.01897055318671));
#30399=CARTESIAN_POINT('Ctrl Pts',(-11.6782764355039,0.868229922828961,
5.05388354529751));
#30400=CARTESIAN_POINT('Ctrl Pts',(-11.539017791421,-1.66098376324763,4.85146318408707));
#30401=CARTESIAN_POINT('Ctrl Pts',(-11.3997591473382,-3.78354173769753,
3.461267687918));
#30402=CARTESIAN_POINT('Ctrl Pts',(-11.2845500715343,-4.77319465007402,
1.6100852481797));
#30403=CARTESIAN_POINT('Ctrl Pts',(-11.215760543758,-4.91786607927562,0.395122348313753));
#30404=CARTESIAN_POINT('Ctrl Pts',(-11.1933905640093,-4.91782725633716,
1.3942835367757E-5));
#30405=CARTESIAN_POINT('Ctrl Pts',(-12.5981094359908,-4.9178331468155,-2.64215081003175E-5));
#30406=CARTESIAN_POINT('Ctrl Pts',(-12.576498946479,-4.91790431974439,-0.381719067368811));
#30407=CARTESIAN_POINT('Ctrl Pts',(-12.5084689089396,-4.77978222981794,
-1.58324067107775));
#30408=CARTESIAN_POINT('Ctrl Pts',(-12.3940193233725,-3.81173006932457,
-3.43020056145098));
#30409=CARTESIAN_POINT('Ctrl Pts',(-12.2547606792897,-1.70061563003689,
-4.83771314693687));
#30410=CARTESIAN_POINT('Ctrl Pts',(-12.1155020352069,0.826857520598954,
-5.06081699469566));
#30411=CARTESIAN_POINT('Ctrl Pts',(-11.9762433911241,3.1518926095914,-4.04488998500265));
#30412=CARTESIAN_POINT('Ctrl Pts',(-11.8369847470412,4.70525541587707,-2.03865972750019));
#30413=CARTESIAN_POINT('Ctrl Pts',(-11.6977261029584,5.10663887602661,0.466691978745618));
#30414=CARTESIAN_POINT('Ctrl Pts',(-11.5584674588755,4.25777298871062,2.85778431477567));
#30415=CARTESIAN_POINT('Ctrl Pts',(-11.4192088147927,2.36648408499891,4.54921038078241));
#30416=CARTESIAN_POINT('Ctrl Pts',(-11.2799501707098,-0.104186924024186,
5.12686133009603));
#30417=CARTESIAN_POINT('Ctrl Pts',(-11.140691526627,-2.54935003304931,4.44931190434692));
#30418=CARTESIAN_POINT('Ctrl Pts',(-11.0014328825442,-4.37036029072556,
2.68244532887828));
#30419=CARTESIAN_POINT('Ctrl Pts',(-10.9039055189988,-4.89632593945952,
0.985115881753022));
#30420=CARTESIAN_POINT('Ctrl Pts',(-10.852797703481,-4.91863020361453,0.0828516383189645));
#30421=CARTESIAN_POINT('Ctrl Pts',(-10.8481094359908,-4.91856570422813,
8.11450425238988E-5));
#30422=CARTESIAN_POINT('Origin',(-62.8183905640093,0.,0.));
#30423=CARTESIAN_POINT('',(-14.6933905640093,-4.91797489380483,0.000101859666493039));
#30424=CARTESIAN_POINT('',(-14.3481094359907,-4.9186636817339,-2.79553420690082E-5));
#30425=CARTESIAN_POINT('',(-62.8183905640093,-4.91825,1.40632325245411E-12));
#30426=CARTESIAN_POINT('Ctrl Pts',(-14.6933905640093,-4.91797489380483,
0.000101859666493224));
#30427=CARTESIAN_POINT('Ctrl Pts',(-14.663163029754,-4.91757672879938,-0.533744249622919));
#30428=CARTESIAN_POINT('Ctrl Pts',(-14.5865159474711,-4.69793048423044,
-1.88772206019698));
#30429=CARTESIAN_POINT('Ctrl Pts',(-14.4634493171606,-3.47740377609158,
-3.76871663386205));
#30430=CARTESIAN_POINT('Ctrl Pts',(-14.3241906730778,-1.2449244032235,-4.9745075453338));
#30431=CARTESIAN_POINT('Ctrl Pts',(-14.184932028995,1.29234760538017,-4.96239858890765));
#30432=CARTESIAN_POINT('Ctrl Pts',(-14.0456733849121,3.51321643969437,-3.73535437892922));
#30433=CARTESIAN_POINT('Ctrl Pts',(-13.9064147408293,4.87395071821435,-1.59378997510416));
#30434=CARTESIAN_POINT('Ctrl Pts',(-13.7671560967465,5.04140427864135,0.937979204258423));
#30435=CARTESIAN_POINT('Ctrl Pts',(-13.6278974526636,3.97457976249027,3.24010459706584));
#30436=CARTESIAN_POINT('Ctrl Pts',(-13.4886388085808,1.93466592572345,4.74896092257761));
#30437=CARTESIAN_POINT('Ctrl Pts',(-13.3493801644979,-0.57890874156636,
5.09513756019038));
#30438=CARTESIAN_POINT('Ctrl Pts',(-13.2101215204151,-2.95075020743805,
4.1938806971144));
#30439=CARTESIAN_POINT('Ctrl Pts',(-13.0747916535855,-4.55363129933737,
2.32023741237006));
#30440=CARTESIAN_POINT('Ctrl Pts',(-12.9858813347836,-4.91807722756079,
0.750083505076204));
#30441=CARTESIAN_POINT('Ctrl Pts',(-12.9433905640093,-4.91859595699376,
-6.98021618345673E-5));
#30442=CARTESIAN_POINT('Ctrl Pts',(-14.3481094359907,-4.9186636817339,-2.79553420692337E-5));
#30443=CARTESIAN_POINT('Ctrl Pts',(-14.3466197375046,-4.91867186760678,
-0.0263267848127573));
#30444=CARTESIAN_POINT('Ctrl Pts',(-14.2987104909908,-4.9120309881119,-0.872102582125515));
#30445=CARTESIAN_POINT('Ctrl Pts',(-14.2043816964495,-4.46016506967744,
-2.5303141236615));
#30446=CARTESIAN_POINT('Ctrl Pts',(-14.0651230523666,-2.70109609887331,
-4.35885786391608));
#30447=CARTESIAN_POINT('Ctrl Pts',(-13.9258644082838,-0.280722556306372,
-5.12023015689262));
#30448=CARTESIAN_POINT('Ctrl Pts',(-13.7866057642009,2.20837979230334,-4.62802557319187));
#30449=CARTESIAN_POINT('Ctrl Pts',(-13.6473471201181,4.15680842943421,-3.00274968889455));
#30450=CARTESIAN_POINT('Ctrl Pts',(-13.5080884760352,5.08753302431593,-0.642315918895402));
#30451=CARTESIAN_POINT('Ctrl Pts',(-13.3688298319524,4.7726859235525,1.87537491939491));
#30452=CARTESIAN_POINT('Ctrl Pts',(-13.2295711878696,3.28935058494016,3.93392103918285));
#30453=CARTESIAN_POINT('Ctrl Pts',(-13.0903125437867,1.00068937108082,5.02933224153838));
#30454=CARTESIAN_POINT('Ctrl Pts',(-12.9510538997039,-1.5329688483594,4.89342094276911));
#30455=CARTESIAN_POINT('Ctrl Pts',(-12.8117952556211,-3.69131302095292,
3.55946206532884));
#30456=CARTESIAN_POINT('Ctrl Pts',(-12.69414710105,-4.75122672230175,1.69628807645834));
#30457=CARTESIAN_POINT('Ctrl Pts',(-12.6229184945066,-4.91775143957992,
0.438160560839145));
#30458=CARTESIAN_POINT('Ctrl Pts',(-12.5981094359908,-4.9178331468155,-2.64215081003175E-5));
#30459=CARTESIAN_POINT('Origin',(-62.8183905640093,0.,0.));
#30460=CARTESIAN_POINT('',(-16.4433905640093,-4.91828387020536,-0.000128019577716025));
#30461=CARTESIAN_POINT('',(-16.0981094359907,-4.91789060884963,7.19626684395069E-5));
#30462=CARTESIAN_POINT('',(-62.8183905640093,-4.91825,1.40632325245411E-12));
#30463=CARTESIAN_POINT('Ctrl Pts',(-16.4433905640093,-4.91828387020536,
-0.000128019577716378));
#30464=CARTESIAN_POINT('Ctrl Pts',(-16.4332838207796,-4.91846947797415,
-0.178590220560657));
#30465=CARTESIAN_POINT('Ctrl Pts',(-16.3767575295224,-4.86519987727275,
-1.17660631794529));
#30466=CARTESIAN_POINT('Ctrl Pts',(-16.2738116902375,-4.20645144279858,
-2.93280213238163));
#30467=CARTESIAN_POINT('Ctrl Pts',(-16.1345530461547,-2.28548001951246,
-4.5904404111952));
#30468=CARTESIAN_POINT('Ctrl Pts',(-15.9952944020718,0.195041427264702,
-5.1242092980259));
#30469=CARTESIAN_POINT('Ctrl Pts',(-15.856035757989,2.62781122700226,-4.40342710210641));
#30470=CARTESIAN_POINT('Ctrl Pts',(-15.7167771139062,4.41721866030238,-2.60456165129585));
#30471=CARTESIAN_POINT('Ctrl Pts',(-15.5775184698233,5.12516627595581,-0.16802598647164));
#30472=CARTESIAN_POINT('Ctrl Pts',(-15.4382598257405,4.57832851364817,2.30964718289191));
#30473=CARTESIAN_POINT('Ctrl Pts',(-15.2990011816576,2.91058669377287,4.22185352497654));
#30474=CARTESIAN_POINT('Ctrl Pts',(-15.1597425375748,0.530251090985978,
5.10043094932504));
#30475=CARTESIAN_POINT('Ctrl Pts',(-15.020483893492,-1.97990494684484,4.73027890190248));
#30476=CARTESIAN_POINT('Ctrl Pts',(-14.8812252494091,-4.00532436477151,
3.20202105259979));
#30477=CARTESIAN_POINT('Ctrl Pts',(-14.7721941395816,-4.82334198966169,
1.39170572320378));
#30478=CARTESIAN_POINT('Ctrl Pts',(-14.7095825777816,-4.91818817925502,
0.286067743649002));
#30479=CARTESIAN_POINT('Ctrl Pts',(-14.6933905640093,-4.91797489380483,
0.000101859666493224));
#30480=CARTESIAN_POINT('Ctrl Pts',(-16.0981094359907,-4.91789060884963,
7.19626684395069E-5));
#30481=CARTESIAN_POINT('Ctrl Pts',(-16.0703209805026,-4.9176377461804,-0.490721850450886));
#30482=CARTESIAN_POINT('Ctrl Pts',(-15.9961129769868,-4.72269515954724,
-1.80156433640869));
#30483=CARTESIAN_POINT('Ctrl Pts',(-15.8754854254435,-3.57520314867229,
-3.6760691586116));
#30484=CARTESIAN_POINT('Ctrl Pts',(-15.7362267813606,-1.37516875424451,
-4.94008835047726));
#30485=CARTESIAN_POINT('Ctrl Pts',(-15.5969681372778,1.16154576959681,-4.99463446493368));
#30486=CARTESIAN_POINT('Ctrl Pts',(-15.457709493195,3.41388110083322,-3.82635307342976));
#30487=CARTESIAN_POINT('Ctrl Pts',(-15.3184508491121,4.83040197127458,-1.72127243894698));
#30488=CARTESIAN_POINT('Ctrl Pts',(-15.1791922050293,5.06430408617135,0.805224276807312));
#30489=CARTESIAN_POINT('Ctrl Pts',(-15.0399335609465,4.05832160518909,3.13457935966327));
#30490=CARTESIAN_POINT('Ctrl Pts',(-14.9006749168636,2.05874743662691,4.69650093211465));
#30491=CARTESIAN_POINT('Ctrl Pts',(-14.7614162727808,-0.444866218910259,
5.10858650317719));
#30492=CARTESIAN_POINT('Ctrl Pts',(-14.622157628698,-2.83956406633868,4.26994589267004));
#30493=CARTESIAN_POINT('Ctrl Pts',(-14.4843886831012,-4.52087640940268,
2.40605627265036));
#30494=CARTESIAN_POINT('Ctrl Pts',(-14.3930392855322,-4.9184167928232,0.793154331015322));
#30495=CARTESIAN_POINT('Ctrl Pts',(-14.3481094359907,-4.9186636817339,-2.79553420692337E-5));
#30496=CARTESIAN_POINT('Origin',(-62.8183905640093,0.,0.));
#30497=CARTESIAN_POINT('',(-18.1933905640093,-4.91828910572115,0.00012777880011387));
#30498=CARTESIAN_POINT('',(-17.8481094359907,-4.91841983696433,-0.000114968478700239));
#30499=CARTESIAN_POINT('',(-62.8183905640093,-4.91825,1.40632325245411E-12));
#30500=CARTESIAN_POINT('Ctrl Pts',(-18.1933905640093,-4.91828910572115,
0.000127778800113817));
#30501=CARTESIAN_POINT('Ctrl Pts',(-18.1569850637777,-4.91762032632294,
-0.642708953241472));
#30502=CARTESIAN_POINT('Ctrl Pts',(-18.0741600155184,-4.62942297978745,
-2.10578920461358));
#30503=CARTESIAN_POINT('Ctrl Pts',(-17.9449154192316,-3.21910722095246,
-3.99160503912099));
#30504=CARTESIAN_POINT('Ctrl Pts',(-17.8056567751488,-0.911389954514629,
-5.04627887052769));
#30505=CARTESIAN_POINT('Ctrl Pts',(-17.6663981310659,1.61946129957759,-4.86548118766222));
#30506=CARTESIAN_POINT('Ctrl Pts',(-17.5271394869831,3.75382271324905,-3.49347636686155));
#30507=CARTESIAN_POINT('Ctrl Pts',(-17.3878808429002,4.96914236350674,-1.26616991732043));
#30508=CARTESIAN_POINT('Ctrl Pts',(-17.2486221988174,4.96787569382644,1.27113066952724));
#30509=CARTESIAN_POINT('Ctrl Pts',(-17.1093635547345,3.75033282070164,3.49722258689558));
#30510=CARTESIAN_POINT('Ctrl Pts',(-16.9701049106517,1.61460260837161,4.86709569511061));
#30511=CARTESIAN_POINT('Ctrl Pts',(-16.8308462665689,-0.916427899620469,
5.0453663883926));
#30512=CARTESIAN_POINT('Ctrl Pts',(-16.691587622486,-3.22309098878473,3.98838896878665));
#30513=CARTESIAN_POINT('Ctrl Pts',(-16.5624357216328,-4.63051303268699,
2.1025194946162));
#30514=CARTESIAN_POINT('Ctrl Pts',(-16.4797033688073,-4.9176169947813,0.641073890954786));
#30515=CARTESIAN_POINT('Ctrl Pts',(-16.4433905640093,-4.91828387020536,
-0.000128019577716378));
#30516=CARTESIAN_POINT('Ctrl Pts',(-17.8481094359907,-4.91841983696433,
-0.000114968478700378));
#30517=CARTESIAN_POINT('Ctrl Pts',(-17.8404417715282,-4.91855474342418,
-0.135497772287647));
#30518=CARTESIAN_POINT('Ctrl Pts',(-17.7863545590381,-4.87991970941729,
-1.09040259937276));
#30519=CARTESIAN_POINT('Ctrl Pts',(-17.6858477985204,-4.28204082740422,
-2.82129196745304));
#30520=CARTESIAN_POINT('Ctrl Pts',(-17.5465891544375,-2.40527633894355,
-4.52881968580006));
#30521=CARTESIAN_POINT('Ctrl Pts',(-17.4073305103547,0.0603676936250531,
-5.12756450517573));
#30522=CARTESIAN_POINT('Ctrl Pts',(-17.2680718662719,2.51123201073006,-4.4709367923799));
#30523=CARTESIAN_POINT('Ctrl Pts',(-17.128813222189,4.34727584434856,-2.71969754684507));
#30524=CARTESIAN_POINT('Ctrl Pts',(-16.9895545781062,5.11898383601734,-0.302599570000859));
#30525=CARTESIAN_POINT('Ctrl Pts',(-16.8502959340234,4.63742008554047,2.18858332338469));
#30526=CARTESIAN_POINT('Ctrl Pts',(-16.7110372899405,3.02048499265497,4.14393923969909));
#30527=CARTESIAN_POINT('Ctrl Pts',(-16.5717786458577,0.664049911073469,
5.08474185468397));
#30528=CARTESIAN_POINT('Ctrl Pts',(-16.4325200017749,-1.85496333359322,
4.78065613113894));
#30529=CARTESIAN_POINT('Ctrl Pts',(-16.293261357692,-3.91982919214168,3.30613083794419));
#30530=CARTESIAN_POINT('Ctrl Pts',(-16.1817911690973,-4.80447615881922,
1.47792554344552));
#30531=CARTESIAN_POINT('Ctrl Pts',(-16.1167405285302,-4.91806014356135,
0.329130371615684));
#30532=CARTESIAN_POINT('Ctrl Pts',(-16.0981094359907,-4.91789060884963,
7.19626684395069E-5));
#30533=CARTESIAN_POINT('Origin',(-62.8183905640093,0.,0.));
#30534=CARTESIAN_POINT('',(-19.9433905640093,-4.91797114886923,-0.000100888655958004));
#30535=CARTESIAN_POINT('',(-19.5981094359907,-4.91815380942886,0.000127431703268871));
#30536=CARTESIAN_POINT('',(-62.8183905640093,-4.91825,1.40632325245411E-12));
#30537=CARTESIAN_POINT('Ctrl Pts',(-19.9433905640093,-4.91797114886923,
-0.000100888655957566));
#30538=CARTESIAN_POINT('Ctrl Pts',(-19.9271058548033,-4.91818339028267,
-0.287704486859558));
#30539=CARTESIAN_POINT('Ctrl Pts',(-19.8644015975697,-4.8226470466571,-1.39498245192419));
#30540=CARTESIAN_POINT('Ctrl Pts',(-19.7552777923085,-4.00212534708821,
-3.20601852685208));
#30541=CARTESIAN_POINT('Ctrl Pts',(-19.6160191482256,-1.97518106715403,
-4.7322533575751));
#30542=CARTESIAN_POINT('Ctrl Pts',(-19.4767605041428,0.535343293589886,
-5.09989898393416));
#30543=CARTESIAN_POINT('Ctrl Pts',(-19.3375018600599,2.91480050434934,-4.21894537866626));
#30544=CARTESIAN_POINT('Ctrl Pts',(-19.1982432159771,4.5806322724203,-2.30507485197035));
#30545=CARTESIAN_POINT('Ctrl Pts',(-19.0589845718943,5.12499595774547,0.17314306632675));
#30546=CARTESIAN_POINT('Ctrl Pts',(-18.9197259278114,4.41461596381525,2.60897067449063));
#30547=CARTESIAN_POINT('Ctrl Pts',(-18.7804672837286,2.6234133658075,4.40604861530454));
#30548=CARTESIAN_POINT('Ctrl Pts',(-18.6412086396458,0.189925121925963,
5.12440148079616));
#30549=CARTESIAN_POINT('Ctrl Pts',(-18.5019499955629,-2.29006215302471,
4.58815621177052));
#30550=CARTESIAN_POINT('Ctrl Pts',(-18.3626913514801,-4.20937756885579,
2.92860078725975));
#30551=CARTESIAN_POINT('Ctrl Pts',(-18.2598382076289,-4.86578064424309,
1.17333004967791));
#30552=CARTESIAN_POINT('Ctrl Pts',(-18.2034046118053,-4.9184730666286,0.176952646436098));
#30553=CARTESIAN_POINT('Ctrl Pts',(-18.1933905640093,-4.91828910572115,
0.000127778800113817));
#30554=CARTESIAN_POINT('Ctrl Pts',(-19.5981094359907,-4.91815380942886,
0.00012743170326894));
#30555=CARTESIAN_POINT('Ctrl Pts',(-19.5641430145262,-4.91756248201972,
-0.599688267675223));
#30556=CARTESIAN_POINT('Ctrl Pts',(-19.4837570450341,-4.65747068326959,
-2.01972912110533));
#30557=CARTESIAN_POINT('Ctrl Pts',(-19.3569515275144,-3.32285072098886,
-3.90566576900731));
#30558=CARTESIAN_POINT('Ctrl Pts',(-19.2176928834316,-1.04363474385184,
-5.02059643215792));
#30559=CARTESIAN_POINT('Ctrl Pts',(-19.0784342393487,1.49109247838584,-4.90634336691521));
#30560=CARTESIAN_POINT('Ctrl Pts',(-18.9391755952659,3.66075817123595,-3.59087894879527));
#30561=CARTESIAN_POINT('Ctrl Pts',(-18.7999169511831,4.93416692759049,-1.39626600038956));
#30562=CARTESIAN_POINT('Ctrl Pts',(-18.6606583071003,4.99955233800879,1.14019227882075));
#30563=CARTESIAN_POINT('Ctrl Pts',(-18.5213996630174,3.84090620831584,3.39749930273613));
#30564=CARTESIAN_POINT('Ctrl Pts',(-18.3821410189346,1.74189781741689,4.82300259245731));
#30565=CARTESIAN_POINT('Ctrl Pts',(-18.2428823748517,-0.783576329617824,
5.0676987034387));
#30566=CARTESIAN_POINT('Ctrl Pts',(-18.1036237307689,-3.11720887230625,
4.0716791204105));
#30567=CARTESIAN_POINT('Ctrl Pts',(-17.9720327511486,-4.60119067126923,
2.18852680733519));
#30568=CARTESIAN_POINT('Ctrl Pts',(-17.8868613195558,-4.91773802838363,
0.68410102396266));
#30569=CARTESIAN_POINT('Ctrl Pts',(-17.8481094359907,-4.91841983696433,
-0.000114968478700378));
#30570=CARTESIAN_POINT('Origin',(-62.8183905640093,0.,0.));
#30571=CARTESIAN_POINT('',(-21.6933905640093,-4.91859939228904,6.83533682649098E-5));
#30572=CARTESIAN_POINT('',(-21.3481094359907,-4.9180816331187,-0.00012121564703732));
#30573=CARTESIAN_POINT('',(-62.8183905640093,-4.91825,1.40632325245411E-12));
#30574=CARTESIAN_POINT('Ctrl Pts',(-21.6933905640093,-4.91859939228904,
6.83533682647487E-5));
#30575=CARTESIAN_POINT('Ctrl Pts',(-21.6508070978013,-4.9180883067121,-0.751719922183042));
#30576=CARTESIAN_POINT('Ctrl Pts',(-21.5618040835657,-4.55241160406376,
-2.32350050460025));
#30577=CARTESIAN_POINT('Ctrl Pts',(-21.4263815213025,-2.94656140448722,
-4.19682474948749));
#30578=CARTESIAN_POINT('Ctrl Pts',(-21.2871228772196,-0.573821271236779,
-5.09571302537738));
#30579=CARTESIAN_POINT('Ctrl Pts',(-21.1478642331369,1.93940650708562,-4.74702691045655));
#30580=CARTESIAN_POINT('Ctrl Pts',(-21.008605589054,3.97781282675011,-3.23613460839731));
#30581=CARTESIAN_POINT('Ctrl Pts',(-20.8693469449712,5.04233828040476,-0.932945204333682));
#30582=CARTESIAN_POINT('Ctrl Pts',(-20.7300883008883,4.87235698748461,1.59865552100332));
#30583=CARTESIAN_POINT('Ctrl Pts',(-20.5908296568055,3.50948516674211,3.73886024782176));
#30584=CARTESIAN_POINT('Ctrl Pts',(-20.4515710127226,1.28739231115071,4.96368644512469));
#30585=CARTESIAN_POINT('Ctrl Pts',(-20.3123123686398,-1.24989052282436,
4.97326208531968));
#30586=CARTESIAN_POINT('Ctrl Pts',(-20.173053724557,-3.48116487480147,3.76524278138513));
#30587=CARTESIAN_POINT('Ctrl Pts',(-20.0500797896801,-4.69889501505713,
1.8844482318336));
#30588=CARTESIAN_POINT('Ctrl Pts',(-19.9735254028309,-4.91757839633652,
0.532109294943383));
#30589=CARTESIAN_POINT('Ctrl Pts',(-19.9433905640093,-4.91797114886923,
-0.000100888655957566));
#30590=CARTESIAN_POINT('Ctrl Pts',(-21.3481094359907,-4.9180816331187,-0.000121215647037425));
#30591=CARTESIAN_POINT('Ctrl Pts',(-21.3342638055519,-4.91830558366444,
-0.244632590468481));
#30592=CARTESIAN_POINT('Ctrl Pts',(-21.2739986270854,-4.84035702823606,
-1.30876342941487));
#30593=CARTESIAN_POINT('Ctrl Pts',(-21.1673139005913,-4.08496228675852,
-3.0997814647056));
#30594=CARTESIAN_POINT('Ctrl Pts',(-21.0280552565085,-2.09880971056153,
-4.67873485164786));
#30595=CARTESIAN_POINT('Ctrl Pts',(-20.8887966124256,0.401190728150701,
-5.11220187520187));
#30596=CARTESIAN_POINT('Ctrl Pts',(-20.7495379683428,2.80296835176735,-4.29405757205957));
#30597=CARTESIAN_POINT('Ctrl Pts',(-20.61027932426,4.51850020045465,-2.4246067622736));
#30598=CARTESIAN_POINT('Ctrl Pts',(-20.4710206801771,5.12777565148253,0.0384562249122501));
#30599=CARTESIAN_POINT('Ctrl Pts',(-20.3317620360943,4.48162687576275,2.49210404269421));
#30600=CARTESIAN_POINT('Ctrl Pts',(-20.1925033920114,2.7382493331312,4.33561444351065));
#30601=CARTESIAN_POINT('Ctrl Pts',(-20.0532447479286,0.324471058226111,
5.11764404248138));
#30602=CARTESIAN_POINT('Ctrl Pts',(-19.9139861038458,-2.16874689092793,
4.64672991858383));
#30603=CARTESIAN_POINT('Ctrl Pts',(-19.774727459763,-4.13099438162065,3.03816514234996));
#30604=CARTESIAN_POINT('Ctrl Pts',(-19.6694352371446,-4.84993378643301,
1.25954143487284));
#30605=CARTESIAN_POINT('Ctrl Pts',(-19.6105625625539,-4.91837060810086,
0.220038169922159));
#30606=CARTESIAN_POINT('Ctrl Pts',(-19.5981094359907,-4.91815380942886,
0.00012743170326894));
#30607=CARTESIAN_POINT('Origin',(-62.8183905640093,0.,0.));
#30608=CARTESIAN_POINT('',(-23.4433905640093,-4.91782678713688,-1.24087024978041E-5));
#30609=CARTESIAN_POINT('',(-23.0981094359907,-4.91849236054295,0.000101443248962593));
#30610=CARTESIAN_POINT('',(-62.8183905640093,-4.91825,1.40632325245411E-12));
#30611=CARTESIAN_POINT('Ctrl Pts',(-23.4433905640093,-4.91782678713688,
-1.24087024978153E-5));
#30612=CARTESIAN_POINT('Ctrl Pts',(-23.4209278888269,-4.91786147762014,
-0.396758149880408));
#30613=CARTESIAN_POINT('Ctrl Pts',(-23.352045665617,-4.77238244581433,-1.61336155032251));
#30614=CARTESIAN_POINT('Ctrl Pts',(-23.2367438943794,-3.78008398872379,
-3.46504359662597));
#30615=CARTESIAN_POINT('Ctrl Pts',(-23.0974852502966,-1.65613904746037,
-4.85311915615117));
#30616=CARTESIAN_POINT('Ctrl Pts',(-22.9582266062137,0.873275482247959,
-5.05301415201156));
#30617=CARTESIAN_POINT('Ctrl Pts',(-22.8189679621309,3.18888752301124,-4.01578864656841));
#30618=CARTESIAN_POINT('Ctrl Pts',(-22.679709318048,4.72376988196712,-1.99538472243945));
#30619=CARTESIAN_POINT('Ctrl Pts',(-22.5404506739652,5.10214003086018,0.513545707623582));
#30620=CARTESIAN_POINT('Ctrl Pts',(-22.4011920298823,4.23136227657829,2.89674565205072));
#30621=CARTESIAN_POINT('Ctrl Pts',(-22.2619333857996,2.32462759375435,4.57074049128587));
#30622=CARTESIAN_POINT('Ctrl Pts',(-22.1226747417167,-0.151241543795875,
5.12568903502298));
#30623=CARTESIAN_POINT('Ctrl Pts',(-21.9834160976339,-2.59008248216644,
4.42572421462287));
#30624=CARTESIAN_POINT('Ctrl Pts',(-21.844157453551,-4.39479811584537,2.64221717678288));
#30625=CARTESIAN_POINT('Ctrl Pts',(-21.7474822756762,-4.90070245514728,
0.955004116442912));
#30626=CARTESIAN_POINT('Ctrl Pts',(-21.6972266458289,-4.91864543283634,
0.0677923221493221));
#30627=CARTESIAN_POINT('Ctrl Pts',(-21.6933905640093,-4.91859939228904,
6.83533682647487E-5));
#30628=CARTESIAN_POINT('Ctrl Pts',(-23.0981094359907,-4.91849236054295,
0.00010144324896242));
#30629=CARTESIAN_POINT('Ctrl Pts',(-23.0579650485499,-4.91784091118313,
-0.708670863612696));
#30630=CARTESIAN_POINT('Ctrl Pts',(-22.9714011130814,-4.58384955508688,
-2.23760099730615));
#30631=CARTESIAN_POINT('Ctrl Pts',(-22.8384176295854,-3.05578981514007,
-4.11797409157195));
#30632=CARTESIAN_POINT('Ctrl Pts',(-22.6991589855025,-0.707481122127949,
-5.0788810258761));
#30633=CARTESIAN_POINT('Ctrl Pts',(-22.5599003414197,1.81403892041534,-4.79633451798247));
#30634=CARTESIAN_POINT('Ctrl Pts',(-22.4206416973369,3.89143102840395,-3.33950992876898));
#30635=CARTESIAN_POINT('Ctrl Pts',(-22.281383053254,5.01609097301024,-1.06507904103722));
#30636=CARTESIAN_POINT('Ctrl Pts',(-22.1421244091712,4.91267025280302,1.47011326107748));
#30637=CARTESIAN_POINT('Ctrl Pts',(-22.0028657650884,3.60648917945748,3.64538033840472));
#30638=CARTESIAN_POINT('Ctrl Pts',(-21.8636071210055,1.41733775071325,4.92815540680027));
#30639=CARTESIAN_POINT('Ctrl Pts',(-21.7243484769227,-1.11881796813,5.00437891924276));
#30640=CARTESIAN_POINT('Ctrl Pts',(-21.5850898328398,-3.38105546629115,
3.85538920824271));
#30641=CARTESIAN_POINT('Ctrl Pts',(-21.4596768191959,-4.67289564265827,
1.97057534616266));
#30642=CARTESIAN_POINT('Ctrl Pts',(-21.3806833535795,-4.91755475594594,
0.575128384443069));
#30643=CARTESIAN_POINT('Ctrl Pts',(-21.3481094359907,-4.9180816331187,-0.000121215647037425));
#30644=CARTESIAN_POINT('Origin',(-62.8183905640093,0.,0.));
#30645=CARTESIAN_POINT('',(-25.1933905640093,-4.9186458426816,-4.33410623697303E-5));
#30646=CARTESIAN_POINT('',(-24.8481094359907,-4.91785710431715,-5.1574967852297E-5));
#30647=CARTESIAN_POINT('',(-62.8183905640093,-4.91825,1.40632325245411E-12));
#30648=CARTESIAN_POINT('Ctrl Pts',(-25.1933905640093,-4.9186458426816,-4.33410623697228E-5));
#30649=CARTESIAN_POINT('Ctrl Pts',(-25.1910486798525,-4.91866493426688,
-0.0413869169074745));
#30650=CARTESIAN_POINT('Ctrl Pts',(-25.1422872476682,-4.90803869591004,
-0.902210422761663));
#30651=CARTESIAN_POINT('Ctrl Pts',(-25.0471062674563,-4.43675165169258,
-2.57114699492807));
#30652=CARTESIAN_POINT('Ctrl Pts',(-24.9078476233734,-2.6609727408645,-4.38346736735891));
#30653=CARTESIAN_POINT('Ctrl Pts',(-24.7685889792906,-0.233712588919614,
-5.12259119138986));
#30654=CARTESIAN_POINT('Ctrl Pts',(-24.6293303352077,2.25076700205062,-4.60756009085119));
#30655=CARTESIAN_POINT('Ctrl Pts',(-24.490071691125,4.18419529608634,-2.96446821749421));
#30656=CARTESIAN_POINT('Ctrl Pts',(-24.3508130470421,5.09321446983781,-0.595590843246681));
#30657=CARTESIAN_POINT('Ctrl Pts',(-24.2115544029592,4.75527096970404,1.91910398181406));
#30658=CARTESIAN_POINT('Ctrl Pts',(-24.0722957588764,3.25310290401414,3.96394797950469));
#30659=CARTESIAN_POINT('Ctrl Pts',(-23.9330371147936,0.954483418570409,
5.03830561716918));
#30660=CARTESIAN_POINT('Ctrl Pts',(-23.7937784707108,-1.57782055097424,
4.8791438180533));
#30661=CARTESIAN_POINT('Ctrl Pts',(-23.6545198266279,-3.72382951079462,
3.52542988341273));
#30662=CARTESIAN_POINT('Ctrl Pts',(-23.5377238577274,-4.75904335759611,
1.66617135078586));
#30663=CARTESIAN_POINT('Ctrl Pts',(-23.4673474368545,-4.91778978907276,
0.423124514933955));
#30664=CARTESIAN_POINT('Ctrl Pts',(-23.4433905640093,-4.91782678713688,
-1.24087024978153E-5));
#30665=CARTESIAN_POINT('Ctrl Pts',(-24.8481094359907,-4.91785710431715,
-5.15749678527133E-5));
#30666=CARTESIAN_POINT('Ctrl Pts',(-24.8280858395755,-4.91798659206747,
-0.353710986347212));
#30667=CARTESIAN_POINT('Ctrl Pts',(-24.7616426951327,-4.79316176184979,
-1.527148550185));
#30668=CARTESIAN_POINT('Ctrl Pts',(-24.6487800026622,-3.86980180875062,
-3.36454989176295));
#30669=CARTESIAN_POINT('Ctrl Pts',(-24.5095213585794,-1.7830527771394,-4.80793976741671));
#30670=CARTESIAN_POINT('Ctrl Pts',(-24.3702627144966,0.740237906473115,
-5.07421026909526));
#30671=CARTESIAN_POINT('Ctrl Pts',(-24.2310040704137,3.08229745508568,-4.09817086168255));
#30672=CARTESIAN_POINT('Ctrl Pts',(-24.0917454263309,4.66972357935212,-2.11878354383227));
#30673=CARTESIAN_POINT('Ctrl Pts',(-23.9524867822481,5.11386955405928,0.379341794741001));
#30674=CARTESIAN_POINT('Ctrl Pts',(-23.8132281381652,4.30599590721036,2.78459355387089));
#30675=CARTESIAN_POINT('Ctrl Pts',(-23.6739694940824,2.44389291227653,4.50809820728166));
#30676=CARTESIAN_POINT('Ctrl Pts',(-23.5347108499995,-0.0165440539888569,
5.12789316459004));
#30677=CARTESIAN_POINT('Ctrl Pts',(-23.3954522059167,-2.47293056883089,
4.49223512462487));
#30678=CARTESIAN_POINT('Ctrl Pts',(-23.2561935618339,-4.32387387433953,
2.75675111897605));
#30679=CARTESIAN_POINT('Ctrl Pts',(-23.1570793051919,-4.88780213881696,
1.04119196874099));
#30680=CARTESIAN_POINT('Ctrl Pts',(-23.1043845965775,-4.91859419169813,
0.110893021562895));
#30681=CARTESIAN_POINT('Ctrl Pts',(-23.0981094359907,-4.91849236054295,
0.00010144324896242));
#30682=CARTESIAN_POINT('Origin',(-62.8183905640093,0.,0.));
#30683=CARTESIAN_POINT('',(-26.9433905640093,-4.91791654477181,8.33642798827967E-5));
#30684=CARTESIAN_POINT('',(-26.5981094359907,-4.91867656610995,1.84189480952973E-6));
#30685=CARTESIAN_POINT('',(-62.8183905640093,-4.91825,1.40632325245411E-12));
#30686=CARTESIAN_POINT('Ctrl Pts',(-26.9433905640093,-4.91791654477181,
8.33642798828485E-5));
#30687=CARTESIAN_POINT('Ctrl Pts',(-26.9147499228506,-4.91761260288967,
-0.5057539384102));
#30688=CARTESIAN_POINT('Ctrl Pts',(-26.8396897336642,-4.71418759851164,
-1.83166998375507));
#30689=CARTESIAN_POINT('Ctrl Pts',(-26.7182099964503,-3.54131022572266,
-3.7087307766292));
#30690=CARTESIAN_POINT('Ctrl Pts',(-26.5789513523675,-1.32976618835693,
-4.95250279885102));
#30691=CARTESIAN_POINT('Ctrl Pts',(-26.4396927082847,1.20734214866586,-4.9837623362656));
#30692=CARTESIAN_POINT('Ctrl Pts',(-26.3004340642018,3.44885904674366,-3.79485617171704));
#30693=CARTESIAN_POINT('Ctrl Pts',(-26.161175420119,4.84599789550719,-1.67686209482602));
#30694=CARTESIAN_POINT('Ctrl Pts',(-26.0219167760362,5.05669966623105,0.851675157476819));
#30695=CARTESIAN_POINT('Ctrl Pts',(-25.8826581319533,4.02937861773551,3.1716982900743));
#30696=CARTESIAN_POINT('Ctrl Pts',(-25.7433994878705,2.01555194199366,4.71520015030647));
#30697=CARTESIAN_POINT('Ctrl Pts',(-25.6041408437876,-0.491738744311117,
5.1042879126934));
#30698=CARTESIAN_POINT('Ctrl Pts',(-25.4648821997048,-2.87863790516758,
4.24370190980198));
#30699=CARTESIAN_POINT('Ctrl Pts',(-25.3279654397787,-4.53247725666741,
2.37608246776745));
#30700=CARTESIAN_POINT('Ctrl Pts',(-25.2374682278802,-4.91828651129618,
0.77810285122316));
#30701=CARTESIAN_POINT('Ctrl Pts',(-25.1933905640093,-4.9186458426816,-4.33410623697228E-5));
#30702=CARTESIAN_POINT('Ctrl Pts',(-26.5981094359907,-4.9186765389473,1.84177752225913E-6));
#30703=CARTESIAN_POINT('Ctrl Pts',(-26.5517870825735,-4.91865835826029,
-0.81775719113905));
#30704=CARTESIAN_POINT('Ctrl Pts',(-26.4590451811287,-4.50155560752193,
-2.45500895652049));
#30705=CARTESIAN_POINT('Ctrl Pts',(-26.3198837316563,-2.77520256653693,
-4.31205435121805));
#30706=CARTESIAN_POINT('Ctrl Pts',(-26.1806250875735,-0.36819586088392,
-5.11468413699221));
#30707=CARTESIAN_POINT('Ctrl Pts',(-26.0413664434906,2.12895558497593,-4.6650948683142));
#30708=CARTESIAN_POINT('Ctrl Pts',(-25.9021077994078,4.10487860730363,-3.07335868919861));
#30709=CARTESIAN_POINT('Ctrl Pts',(-25.762849155325,5.07581147371895,-0.729177547950212));
#30710=CARTESIAN_POINT('Ctrl Pts',(-25.6235905112421,4.80404241095214,1.79352684031905));
#30711=CARTESIAN_POINT('Ctrl Pts',(-25.4843318671593,3.35610815708752,3.87712523025787));
#30712=CARTESIAN_POINT('Ctrl Pts',(-25.3450732230764,1.08650388987611,5.01149392002581));
#30713=CARTESIAN_POINT('Ctrl Pts',(-25.2058145789936,-1.44910719949644,
4.91890743331681));
#30714=CARTESIAN_POINT('Ctrl Pts',(-25.0665559349108,-3.62993594091732,
3.62203355561599));
#30715=CARTESIAN_POINT('Ctrl Pts',(-24.9473208872432,-4.7362640055411,1.75236430941362));
#30716=CARTESIAN_POINT('Ctrl Pts',(-24.8745053876031,-4.91768640808852,
0.466157217721872));
#30717=CARTESIAN_POINT('Ctrl Pts',(-24.8481094359907,-4.91785710431715,
-5.15749678527133E-5));
#30718=CARTESIAN_POINT('Origin',(-62.8183905640093,0.,0.));
#30719=CARTESIAN_POINT('',(-28.6933905640092,-4.91837309484402,-0.000121104502655431));
#30720=CARTESIAN_POINT('',(-28.3481094359907,-4.9178533390618,4.85856934917539E-5));
#30721=CARTESIAN_POINT('',(-62.8183905640093,-4.91825,1.40632325245411E-12));
#30722=CARTESIAN_POINT('Ctrl Pts',(-28.6933905640092,-4.91837309484402,
-0.000121104502655602));
#30723=CARTESIAN_POINT('Ctrl Pts',(-28.6848707138762,-4.91852719604813,
-0.150554503830029));
#30724=CARTESIAN_POINT('Ctrl Pts',(-28.6299313157155,-4.87490927511793,
-1.12052014919942));
#30725=CARTESIAN_POINT('Ctrl Pts',(-28.5285723695273,-4.25596405301566,
-2.86047759434731));
#30726=CARTESIAN_POINT('Ctrl Pts',(-28.3893137254443,-2.36360537794301,
-4.55070672595844));
#30727=CARTESIAN_POINT('Ctrl Pts',(-28.2500550813616,0.107430613693398,
-5.12679439333839));
#30728=CARTESIAN_POINT('Ctrl Pts',(-28.1107964372787,2.55216455853763,-4.44769807366338));
#30729=CARTESIAN_POINT('Ctrl Pts',(-27.9715377931959,4.37205657674479,-2.67967971557556));
#30730=CARTESIAN_POINT('Ctrl Pts',(-27.832279149113,5.12154573019909,-0.255600120899675));
#30731=CARTESIAN_POINT('Ctrl Pts',(-27.6930205050302,4.61713591749465,2.23105759847328));
#30732=CARTESIAN_POINT('Ctrl Pts',(-27.5537618609474,2.98232089930236,4.17148943926614));
#30733=CARTESIAN_POINT('Ctrl Pts',(-27.4145032168645,0.617349539765915,
5.09062291218622));
#30734=CARTESIAN_POINT('Ctrl Pts',(-27.2752445727817,-1.89876641369781,
4.76342819768889));
#30735=CARTESIAN_POINT('Ctrl Pts',(-27.1359859286988,-3.9500107505568,3.27001179796192));
#30736=CARTESIAN_POINT('Ctrl Pts',(-27.0253679257747,-4.81120499508792,
1.44780147547091));
#30737=CARTESIAN_POINT('Ctrl Pts',(-26.9611694708782,-4.91810521912398,
0.314085912111188));
#30738=CARTESIAN_POINT('Ctrl Pts',(-26.9433905640093,-4.91791654477181,
8.33642798828485E-5));
#30739=CARTESIAN_POINT('Ctrl Pts',(-28.3481094359907,-4.91785333906181,
4.85856934917886E-5));
#30740=CARTESIAN_POINT('Ctrl Pts',(-28.3219078735991,-4.91769386938119,
-0.462727892406216));
#30741=CARTESIAN_POINT('Ctrl Pts',(-28.24928676318,-4.73812545833518,-1.74549558120992));
#30742=CARTESIAN_POINT('Ctrl Pts',(-28.1302461047332,-3.63751179343058,
-3.61442526078837));
#30743=CARTESIAN_POINT('Ctrl Pts',(-27.9909874606504,-1.45940322528745,
-4.91586251223447));
#30744=CARTESIAN_POINT('Ctrl Pts',(-27.8517288165675,1.07600844855802,-5.01375785532204));
#30745=CARTESIAN_POINT('Ctrl Pts',(-27.7124701724847,3.34798288054322,-3.88414374666556));
#30746=CARTESIAN_POINT('Ctrl Pts',(-27.5732115284018,4.80027659624061,-1.80358160690233));
#30747=CARTESIAN_POINT('Ctrl Pts',(-27.433952884319,5.07732709858328,0.718548221877666));
#30748=CARTESIAN_POINT('Ctrl Pts',(-27.2946942402362,4.11130460399385,3.06475716270483));
#30749=CARTESIAN_POINT('Ctrl Pts',(-27.1554355961534,2.13871868810873,4.66062703788945));
#30750=CARTESIAN_POINT('Ctrl Pts',(-27.0161769520704,-0.357485934549103,
5.11544385364273));
#30751=CARTESIAN_POINT('Ctrl Pts',(-26.8769183079877,-2.76616790928751,
4.3178556148625));
#30752=CARTESIAN_POINT('Ctrl Pts',(-26.7376596639048,-4.49761389622142,
2.46313443678733));
#30753=CARTESIAN_POINT('Ctrl Pts',(-26.6447233732392,-4.9182559093769,0.822908377436444));
#30754=CARTESIAN_POINT('Ctrl Pts',(-26.5982066306011,-4.91867657709443,
0.00171768228997997));
#30755=CARTESIAN_POINT('Ctrl Pts',(-26.5981094359907,-4.9186765389473,1.84177752225913E-6));
#30756=CARTESIAN_POINT('Origin',(-62.8183905640093,0.,0.));
#30757=CARTESIAN_POINT('',(-30.4433905640093,-4.91820020867345,0.000129117068208339));
#30758=CARTESIAN_POINT('',(-30.0981094359907,-4.91850196224555,-9.92246832554056E-5));
#30759=CARTESIAN_POINT('',(-62.8183905640093,-4.91825,1.40632325245411E-12));
#30760=CARTESIAN_POINT('Ctrl Pts',(-30.4433905640093,-4.91820020867345,
0.000129117068208267));
#30761=CARTESIAN_POINT('Ctrl Pts',(-30.4085719568742,-4.91757590647288,
-0.614718730968464));
#30762=CARTESIAN_POINT('Ctrl Pts',(-30.3273338017115,-4.64782072635045,
-2.04980313689827));
#30763=CARTESIAN_POINT('Ctrl Pts',(-30.1996760985213,-3.28686098148408,
-3.93600139440042));
#30764=CARTESIAN_POINT('Ctrl Pts',(-30.0604174544384,-0.997507167463827,
-5.02996436758579));
#30765=CARTESIAN_POINT('Ctrl Pts',(-29.9211588103556,1.53606455886436,-4.89245007734626));
#30766=CARTESIAN_POINT('Ctrl Pts',(-29.7819001662728,3.69356432102827,-3.55712590369689));
#30767=CARTESIAN_POINT('Ctrl Pts',(-29.6426415221899,4.94677527517285,-1.35091689798559));
#30768=CARTESIAN_POINT('Ctrl Pts',(-29.5033828781071,4.98887600398362,1.18603469814376));
#30769=CARTESIAN_POINT('Ctrl Pts',(-29.3641242340243,3.80955906062489,3.43261152068441));
#30770=CARTESIAN_POINT('Ctrl Pts',(-29.2248655899414,1.6975545226847,4.83878814692659));
#30771=CARTESIAN_POINT('Ctrl Pts',(-29.0856069458586,-0.83005928111469,
5.06029284509897));
#30772=CARTESIAN_POINT('Ctrl Pts',(-28.9463483017757,-3.15445114191686,
4.0428950124365));
#30773=CARTESIAN_POINT('Ctrl Pts',(-28.815609507826,-4.6115871884147,2.15848371842179));
#30774=CARTESIAN_POINT('Ctrl Pts',(-28.7312902619038,-4.91768759110979,
0.669066768371859));
#30775=CARTESIAN_POINT('Ctrl Pts',(-28.6933905640092,-4.91837309484402,
-0.000121104502655602));
#30776=CARTESIAN_POINT('Ctrl Pts',(-30.0981094359907,-4.91850196224555,
-9.92246832555964E-5));
#30777=CARTESIAN_POINT('Ctrl Pts',(-30.0920286646248,-4.91859912603189,
-0.107458143160632));
#30778=CARTESIAN_POINT('Ctrl Pts',(-30.0395283452312,-4.8888725063671,-1.03432258519129));
#30779=CARTESIAN_POINT('Ctrl Pts',(-29.9406084778101,-4.32963647845777,
-2.74769175446946));
#30780=CARTESIAN_POINT('Ctrl Pts',(-29.8013498337272,-2.48233098445573,
-4.48704745871744));
#30781=CARTESIAN_POINT('Ctrl Pts',(-29.6620911896444,-0.0272807940196574,
-5.12784728433378));
#30782=CARTESIAN_POINT('Ctrl Pts',(-29.5228325455616,2.43444850487691,-4.5132053454584));
#30783=CARTESIAN_POINT('Ctrl Pts',(-29.3835739014787,4.30015608997081,-2.79360333889022));
#30784=CARTESIAN_POINT('Ctrl Pts',(-29.2443152573959,5.11306407908685,-0.390048376901321));
#30785=CARTESIAN_POINT('Ctrl Pts',(-29.105056613313,4.67414964965714,2.10900143807006));
#30786=CARTESIAN_POINT('Ctrl Pts',(-28.9657979692302,3.09087144371802,4.09170816793918));
#30787=CARTESIAN_POINT('Ctrl Pts',(-28.8265393251474,0.750860658988233,
5.07264923722855));
#30788=CARTESIAN_POINT('Ctrl Pts',(-28.6872806810645,-1.77298201041712,
4.81166258209249));
#30789=CARTESIAN_POINT('Ctrl Pts',(-28.5480220369817,-3.86274863579312,
3.37264510286066));
#30790=CARTESIAN_POINT('Ctrl Pts',(-28.4349649552904,-4.79155068651975,
1.53401980474453));
#30791=CARTESIAN_POINT('Ctrl Pts',(-28.3683274216268,-4.91797639110214,
0.357142107335489));
#30792=CARTESIAN_POINT('Ctrl Pts',(-28.3481094359907,-4.91785333906181,
4.85856934917886E-5));
#30793=CARTESIAN_POINT('Origin',(-62.8183905640093,0.,0.));
#30794=CARTESIAN_POINT('',(-32.1933905640093,-4.9180404057301,-0.000115405238602364));
#30795=CARTESIAN_POINT('',(-31.8481094359907,-4.91807200796895,0.000120019908876473));
#30796=CARTESIAN_POINT('',(-62.8183905640093,-4.91825,1.40632325245411E-12));
#30797=CARTESIAN_POINT('Ctrl Pts',(-32.1933905640093,-4.9180404057301,-0.000115405238602581));
#30798=CARTESIAN_POINT('Ctrl Pts',(-32.1786927478998,-4.91826392058507,
-0.259682470608151));
#30799=CARTESIAN_POINT('Ctrl Pts',(-32.1175753837628,-4.83430517290801,
-1.33888704426319));
#30800=CARTESIAN_POINT('Ctrl Pts',(-32.0100384715981,-4.0563375838621,-3.13714639347168));
#30801=CARTESIAN_POINT('Ctrl Pts',(-31.8707798275153,-2.05577560156633,
-4.69780254633261));
#30802=CARTESIAN_POINT('Ctrl Pts',(-31.7315211834325,0.448098278592388,
-5.10830402590205));
#30803=CARTESIAN_POINT('Ctrl Pts',(-31.5922625393496,2.84226505119731,-4.26814848231254));
#30804=CARTESIAN_POINT('Ctrl Pts',(-31.4530038952668,4.54056510758199,-2.38302970861326));
#30805=CARTESIAN_POINT('Ctrl Pts',(-31.313745251184,5.12720665419247,0.0855220061093843));
#30806=CARTESIAN_POINT('Ctrl Pts',(-31.1744866071012,4.45856328065359,2.5331355196144));
#30807=CARTESIAN_POINT('Ctrl Pts',(-31.0352279630183,2.69833775932673,4.360565952364));
#30808=CARTESIAN_POINT('Ctrl Pts',(-30.8959693189355,0.277482985620765,
5.12040674956741));
#30809=CARTESIAN_POINT('Ctrl Pts',(-30.7567106748526,-2.21130745577726,
4.62662743522194));
#30810=CARTESIAN_POINT('Ctrl Pts',(-30.6174520307698,-4.15870741103577,
3.00011912392169));
#30811=CARTESIAN_POINT('Ctrl Pts',(-30.513011993822,-4.85560432133482,1.22941940689503));
#30812=CARTESIAN_POINT('Ctrl Pts',(-30.4549915049018,-4.91840821506784,
0.204985489275344));
#30813=CARTESIAN_POINT('Ctrl Pts',(-30.4433905640093,-4.91820020867345,
0.000129117068208267));
#30814=CARTESIAN_POINT('Ctrl Pts',(-31.8481094359907,-4.91807200796895,
0.000120019908876265));
#30815=CARTESIAN_POINT('Ctrl Pts',(-31.8157299076228,-4.91755498663457,
-0.57169991192379));
#30816=CARTESIAN_POINT('Ctrl Pts',(-31.7369308312273,-4.67501516669824,
-1.96371255691315));
#30817=CARTESIAN_POINT('Ctrl Pts',(-31.6117122068041,-3.38912046412381,
-3.84830150752625));
#30818=CARTESIAN_POINT('Ctrl Pts',(-31.4724535627214,-1.12929367800508,
-5.00202536998659));
#30819=CARTESIAN_POINT('Ctrl Pts',(-31.3331949186384,1.40701607828237,-4.93111222429854));
#30820=CARTESIAN_POINT('Ctrl Pts',(-31.1939362745556,3.59884858124293,-3.65292361026856));
#30821=CARTESIAN_POINT('Ctrl Pts',(-31.0546776304728,4.90958136292712,-1.48039618142248));
#30822=CARTESIAN_POINT('Ctrl Pts',(-30.9154189863899,5.01831003890801,1.05457402137864));
#30823=CARTESIAN_POINT('Ctrl Pts',(-30.7761603423071,3.89841476010363,3.33135473514573));
#30824=CARTESIAN_POINT('Ctrl Pts',(-30.6369016982242,1.82407750325954,4.79252577199894));
#30825=CARTESIAN_POINT('Ctrl Pts',(-30.4976430541415,-0.696845416589377,
5.08035121606272));
#30826=CARTESIAN_POINT('Ctrl Pts',(-30.3583844100586,-3.04716090784859,
4.12436327387041));
#30827=CARTESIAN_POINT('Ctrl Pts',(-30.2252065373417,-4.5813938197129,2.24444978973811));
#30828=CARTESIAN_POINT('Ctrl Pts',(-30.1384482126524,-4.91785739463383,
0.712101115451537));
#30829=CARTESIAN_POINT('Ctrl Pts',(-30.0981094359907,-4.91850196224555,
-9.92246832555964E-5));
#30830=CARTESIAN_POINT('Origin',(-62.8183905640093,0.,0.));
#30831=CARTESIAN_POINT('',(-33.9433905640093,-4.91853326571986,9.11492385194351E-5));
#30832=CARTESIAN_POINT('',(-33.5981094359907,-4.91816426918661,-0.000127960998163867));
#30833=CARTESIAN_POINT('',(-62.8183905640093,-4.91825,1.40632325245411E-12));
#30834=CARTESIAN_POINT('Ctrl Pts',(-33.9433905640093,-4.91853326571986,
9.11492385192135E-5));
#30835=CARTESIAN_POINT('Ctrl Pts',(-33.9023939908979,-4.91791720891167,
-0.723709576353512));
#30836=CARTESIAN_POINT('Ctrl Pts',(-33.8149778697589,-4.57302002945823,
-2.26762205719794));
#30837=CARTESIAN_POINT('Ctrl Pts',(-33.6811422005921,-3.01786256635649,
-4.1458494447952));
#30838=CARTESIAN_POINT('Ctrl Pts',(-33.5418835565094,-0.660832717283021,
-5.08516098153175));
#30839=CARTESIAN_POINT('Ctrl Pts',(-33.4026249124265,1.85798763502059,-4.7794815656549));
#30840=CARTESIAN_POINT('Ctrl Pts',(-33.2633662683437,3.92192016684631,-3.30365014691457));
#30841=CARTESIAN_POINT('Ctrl Pts',(-33.1241076242608,5.02565593354922,-1.01899191650671));
#30842=CARTESIAN_POINT('Ctrl Pts',(-32.9848489801781,4.89896926309818,1.51514429924805));
#30843=CARTESIAN_POINT('Ctrl Pts',(-32.8455903360952,3.57287662854112,3.67833042093137));
#30844=CARTESIAN_POINT('Ctrl Pts',(-32.7063316920124,1.37204293986752,4.94095742336282));
#30845=CARTESIAN_POINT('Ctrl Pts',(-32.5670730479295,-1.16470559062442,
4.99389857481034));
#30846=CARTESIAN_POINT('Ctrl Pts',(-32.4278144038467,-3.41630131512815,
3.82419238697246));
#30847=CARTESIAN_POINT('Ctrl Pts',(-32.3032535758732,-4.68212636122256,
1.94048764453586));
#30848=CARTESIAN_POINT('Ctrl Pts',(-32.2251122959274,-4.91755800220454,
0.560098221135963));
#30849=CARTESIAN_POINT('Ctrl Pts',(-32.1933905640093,-4.9180404057301,-0.000115405238602581));
#30850=CARTESIAN_POINT('Ctrl Pts',(-33.5981094359907,-4.91816426918661,
-0.00012796099816411));
#30851=CARTESIAN_POINT('Ctrl Pts',(-33.5858506986484,-4.91837934192607,
-0.21660464215519));
#30852=CARTESIAN_POINT('Ctrl Pts',(-33.5271724132785,-4.85123996273957,
-1.25267033401488));
#30853=CARTESIAN_POINT('Ctrl Pts',(-33.422074579881,-4.13734663286075,-3.02950901182476));
#30854=CARTESIAN_POINT('Ctrl Pts',(-33.2828159357982,-2.17847145432949,
-4.64217881342837));
#30855=CARTESIAN_POINT('Ctrl Pts',(-33.1435572917154,0.313755030289582,
-5.11831220170669));
#30856=CARTESIAN_POINT('Ctrl Pts',(-33.0042986476325,2.72916542679145,-4.34133828287751));
#30857=CARTESIAN_POINT('Ctrl Pts',(-32.8650400035497,4.47639908771296,-2.50148220475266));
#30858=CARTESIAN_POINT('Ctrl Pts',(-32.7257813594668,5.12768389180779,-0.0491926708628662));
#30859=CARTESIAN_POINT('Ctrl Pts',(-32.586522715384,4.52356693451351,2.41514061746884));
#30860=CARTESIAN_POINT('Ctrl Pts',(-32.4472640713011,2.81195310003798,4.28817930785997));
#30861=CARTESIAN_POINT('Ctrl Pts',(-32.3080054272183,0.411893770634228,
5.11135065661556));
#30862=CARTESIAN_POINT('Ctrl Pts',(-32.1687467831355,-2.08900878079138,
4.68311908101302));
#30863=CARTESIAN_POINT('Ctrl Pts',(-32.0294881390527,-4.07846301397088,
3.10832775891526));
#30864=CARTESIAN_POINT('Ctrl Pts',(-31.9226090233377,-4.83898935836676,
1.31563478630209));
#30865=CARTESIAN_POINT('Ctrl Pts',(-31.8621494556504,-4.91829619250977,
0.24806566610592));
#30866=CARTESIAN_POINT('Ctrl Pts',(-31.8481094359907,-4.91807200796895,
0.000120019908876265));
#30867=CARTESIAN_POINT('Origin',(-62.8183905640093,0.,0.));
#30868=CARTESIAN_POINT('',(-35.6933905640092,-4.91784231204611,-3.82622793895393E-5));
#30869=CARTESIAN_POINT('',(-35.3481094359907,-4.91840929431599,0.000116514561900802));
#30870=CARTESIAN_POINT('',(-62.8183905640093,-4.91825,1.40632325245411E-12));
#30871=CARTESIAN_POINT('Ctrl Pts',(-35.6933905640093,-4.91784231204611,
-3.82622793893006E-5));
#30872=CARTESIAN_POINT('Ctrl Pts',(-35.6725147819235,-4.91794209965865,
-0.368752264205334));
#30873=CARTESIAN_POINT('Ctrl Pts',(-35.6052194518101,-4.78604129458979,
-1.55727124936419));
#30874=CARTESIAN_POINT('Ctrl Pts',(-35.4915045736691,-3.8387558835552,-3.39992872789929));
#30875=CARTESIAN_POINT('Ctrl Pts',(-35.3522459295862,-1.73884600907171,
-4.82410371416908));
#30876=CARTESIAN_POINT('Ctrl Pts',(-35.2129872855035,0.786782452717923,
-5.06720193602146));
#30877=CARTESIAN_POINT('Ctrl Pts',(-35.0737286414205,3.11978436072366,-4.06970608655078));
#30878=CARTESIAN_POINT('Ctrl Pts',(-34.9344699973378,4.68897499169966,-2.07583130710078));
#30879=CARTESIAN_POINT('Ctrl Pts',(-34.7952113532549,5.11017218394326,0.426265573061127));
#30880=CARTESIAN_POINT('Ctrl Pts',(-34.6559527091721,4.28025497520489,2.82400060827867));
#30881=CARTESIAN_POINT('Ctrl Pts',(-34.5166940650892,2.40241052515365,4.53034057847261));
#30882=CARTESIAN_POINT('Ctrl Pts',(-34.3774354210064,-0.0636118368933031,
5.12752529223713));
#30883=CARTESIAN_POINT('Ctrl Pts',(-34.2381767769235,-2.51406022562872,
4.46934707426445));
#30884=CARTESIAN_POINT('Ctrl Pts',(-34.0989181328408,-4.34899570403538,
2.71694653142206));
#30885=CARTESIAN_POINT('Ctrl Pts',(-34.0006560618693,-4.89244018058238,
1.01107768639465));
#30886=CARTESIAN_POINT('Ctrl Pts',(-33.9488135389255,-4.91861475693642,
0.0958345951248656));
#30887=CARTESIAN_POINT('Ctrl Pts',(-33.9433905640093,-4.91853326571986,
9.11492385192135E-5));
#30888=CARTESIAN_POINT('Ctrl Pts',(-35.3481094359907,-4.91840929431599,
0.000116514561900646));
#30889=CARTESIAN_POINT('Ctrl Pts',(-35.3095519416465,-4.91772571242185,
-0.68067148944363));
#30890=CARTESIAN_POINT('Ctrl Pts',(-35.2245748992746,-4.60357657753055,
-2.18167446257958));
#30891=CARTESIAN_POINT('Ctrl Pts',(-35.0931783088751,-3.125727316038,-4.06514338725531));
#30892=CARTESIAN_POINT('Ctrl Pts',(-34.9539196647922,-0.794185353227152,
-5.06604694390913));
#30893=CARTESIAN_POINT('Ctrl Pts',(-34.8146610207094,1.73179560238191,-4.82663920391221));
#30894=CARTESIAN_POINT('Ctrl Pts',(-34.6754023766266,3.83378410926193,-3.40553394003679));
#30895=CARTESIAN_POINT('Ctrl Pts',(-34.5361437325437,4.99715404582752,-1.15065783595354));
#30896=CARTESIAN_POINT('Ctrl Pts',(-34.3968850884609,4.93707961190701,1.38593178723334));
#30897=CARTESIAN_POINT('Ctrl Pts',(-34.257626444378,3.6682687247101,3.58320618671119));
#30898=CARTESIAN_POINT('Ctrl Pts',(-34.1183678002952,1.5013621055187,4.90321056464884));
#30899=CARTESIAN_POINT('Ctrl Pts',(-33.9791091562124,-1.03312033767432,
5.02277058813713));
#30900=CARTESIAN_POINT('Ctrl Pts',(-33.8398505121295,-3.31466575920044,
3.91261458847608));
#30901=CARTESIAN_POINT('Ctrl Pts',(-33.712850605389,-4.6552835507772,2.02658970348332));
#30902=CARTESIAN_POINT('Ctrl Pts',(-33.632270246676,-4.91756493673245,0.603116787323793));
#30903=CARTESIAN_POINT('Ctrl Pts',(-33.5981094359907,-4.91816426918661,
-0.00012796099816411));
#30904=CARTESIAN_POINT('Origin',(-62.8183905640093,0.,0.));
#30905=CARTESIAN_POINT('',(-37.4433905640093,-4.91867318169596,-1.4270610707154E-5));
#30906=CARTESIAN_POINT('',(-37.0981094359907,-4.91789617187166,-7.46432797521512E-5));
#30907=CARTESIAN_POINT('',(-62.8183905640093,-4.91825,1.40632325245411E-12));
#30908=CARTESIAN_POINT('Ctrl Pts',(-37.4433905640093,-4.91867318169596,
-1.42706107073378E-5));
#30909=CARTESIAN_POINT('Ctrl Pts',(-37.4426355729491,-4.91867538847336,
-0.0133426519680256));
#30910=CARTESIAN_POINT('Ctrl Pts',(-37.3954610338614,-4.91536146633527,
-0.846146440759592));
#30911=CARTESIAN_POINT('Ctrl Pts',(-37.3018669467459,-4.48004925758386,
-2.49493902489554));
#30912=CARTESIAN_POINT('Ctrl Pts',(-37.1626083026632,-2.7355056920653,-4.33734604303171));
#30913=CARTESIAN_POINT('Ctrl Pts',(-37.0233496585803,-0.321233115053798,
-5.11784831487974));
#30914=CARTESIAN_POINT('Ctrl Pts',(-36.8840910144975,2.17168639631715,-4.64535685221012));
#30915=CARTESIAN_POINT('Ctrl Pts',(-36.7448323704146,4.13291577533089,-3.03555090261152));
#30916=CARTESIAN_POINT('Ctrl Pts',(-36.6055737263318,5.08229070826373,-0.68255640427784));
#30917=CARTESIAN_POINT('Ctrl Pts',(-36.4663150822489,4.78737741250149,1.8375471690803));
#30918=CARTESIAN_POINT('Ctrl Pts',(-36.3270564381661,3.3203789876831,3.90776732501783));
#30919=CARTESIAN_POINT('Ctrl Pts',(-36.1877977940833,1.04045805875398,5.02125573101972));
#30920=CARTESIAN_POINT('Ctrl Pts',(-36.0485391500004,-1.49419637309213,
4.90539899365616));
#30921=CARTESIAN_POINT('Ctrl Pts',(-35.9092805059176,-3.66302935450954,
3.58856211264706));
#30922=CARTESIAN_POINT('Ctrl Pts',(-35.7908976439206,-4.74436522801712,
1.72225148136041));
#30923=CARTESIAN_POINT('Ctrl Pts',(-35.7189343299511,-4.91772021116346,
0.451122998456921));
#30924=CARTESIAN_POINT('Ctrl Pts',(-35.6933905640093,-4.91784231204611,
-3.82622793893006E-5));
#30925=CARTESIAN_POINT('Ctrl Pts',(-37.0981094359907,-4.91789617187166,
-7.46432797522553E-5));
#30926=CARTESIAN_POINT('Ctrl Pts',(-37.0796727326721,-4.91807043539616,
-0.325698736799547));
#30927=CARTESIAN_POINT('Ctrl Pts',(-37.0148164813258,-4.80602407783864,
-1.47105406828722));
#30928=CARTESIAN_POINT('Ctrl Pts',(-36.903540681952,-3.92674297249402,-3.29791625744811));
#30929=CARTESIAN_POINT('Ctrl Pts',(-36.7642820378691,-1.86496899934438,
-4.7767617320373));
#30930=CARTESIAN_POINT('Ctrl Pts',(-36.6250233937863,0.653402029340091,
-5.08612109580827));
#30931=CARTESIAN_POINT('Ctrl Pts',(-36.4857647497035,3.01180179695694,-4.15025444388879));
#30932=CARTESIAN_POINT('Ctrl Pts',(-36.3465061056206,4.63282746729464,-2.19828835038808));
#30933=CARTESIAN_POINT('Ctrl Pts',(-36.2072474615378,5.11960619781114,0.291880784748528));
#30934=CARTESIAN_POINT('Ctrl Pts',(-36.0679888174549,4.35296081444672,2.71058926454433));
#30935=CARTESIAN_POINT('Ctrl Pts',(-35.9287301733721,2.52058774797673,4.46566897764727));
#30936=CARTESIAN_POINT('Ctrl Pts',(-35.7894715292892,0.0711036494477585,
5.12742686775803));
#30937=CARTESIAN_POINT('Ctrl Pts',(-35.6502128852065,-2.39578862958558,
4.53384592322236));
#30938=CARTESIAN_POINT('Ctrl Pts',(-35.5109542411235,-4.27612422358166,
2.83025151491343));
#30939=CARTESIAN_POINT('Ctrl Pts',(-35.410253091385,-4.87878928807346,1.09727250995654));
#30940=CARTESIAN_POINT('Ctrl Pts',(-35.3559714896741,-4.9185486798658,0.138932377093802));
#30941=CARTESIAN_POINT('Ctrl Pts',(-35.3481094359907,-4.91840929431599,
0.000116514561900646));
#30942=CARTESIAN_POINT('Origin',(-62.8183905640093,0.,0.));
#30943=CARTESIAN_POINT('',(-39.1933905640093,-4.91787152802865,6.14470143739343E-5));
#30944=CARTESIAN_POINT('',(-38.8481094359907,-4.91866022846763,3.15193572706859E-5));
#30945=CARTESIAN_POINT('',(-62.8183905640093,-4.91825,1.40632325245411E-12));
#30946=CARTESIAN_POINT('Ctrl Pts',(-39.1933905640093,-4.91787152802865,
6.14470143736612E-5));
#30947=CARTESIAN_POINT('Ctrl Pts',(-39.1663368159471,-4.91766233869729,
-0.477761426883304));
#30948=CARTESIAN_POINT('Ctrl Pts',(-39.0928635198574,-4.72990563556455,
-1.7756065190772));
#30949=CARTESIAN_POINT('Ctrl Pts',(-38.9729706757401,-3.60418206959766,
-3.64766140116037));
#30950=CARTESIAN_POINT('Ctrl Pts',(-38.8337120316572,-1.41421947780232,
-4.92905116193056));
#30951=CARTESIAN_POINT('Ctrl Pts',(-38.6944533875743,1.12198396286053,-5.00367006060634));
#30952=CARTESIAN_POINT('Ctrl Pts',(-38.5551947434916,3.38349405796131,-3.85324928444358));
#30953=CARTESIAN_POINT('Ctrl Pts',(-38.4159360994086,4.81662929812997,-1.75944431361739));
#30954=CARTESIAN_POINT('Ctrl Pts',(-38.2766774553259,5.07051772191601,0.765122290918382));
#30955=CARTESIAN_POINT('Ctrl Pts',(-38.137418811243,4.08300027639372,3.10236536070355));
#30956=CARTESIAN_POINT('Ctrl Pts',(-37.9981601671602,2.09584910794909,4.68006181636883));
#30957=CARTESIAN_POINT('Ctrl Pts',(-37.8589015230773,-0.404425083919172,
5.11194703022454));
#30958=CARTESIAN_POINT('Ctrl Pts',(-37.7196428789945,-2.80568459910014,
4.29228331062813));
#30959=CARTESIAN_POINT('Ctrl Pts',(-37.5811392259718,-4.51073897975614,
2.43188858802557));
#30960=CARTESIAN_POINT('Ctrl Pts',(-37.4890551209767,-4.91853970791323,
0.806133857362442));
#30961=CARTESIAN_POINT('Ctrl Pts',(-37.4433905640093,-4.91867318169596,
-1.42706107073378E-5));
#30962=CARTESIAN_POINT('Ctrl Pts',(-38.8481094359907,-4.91866022846763,
3.15193572706382E-5));
#30963=CARTESIAN_POINT('Ctrl Pts',(-38.8033739756701,-4.91838593018476,
-0.789720674032932));
#30964=CARTESIAN_POINT('Ctrl Pts',(-38.7122189673219,-4.52353751094886,
-2.39922006544932));
#30965=CARTESIAN_POINT('Ctrl Pts',(-38.574644410946,-2.84849824938738,-4.26399105726181));
#30966=CARTESIAN_POINT('Ctrl Pts',(-38.4353857668631,-0.455561595795777,
-5.10764384482783));
#30967=CARTESIAN_POINT('Ctrl Pts',(-38.2961271227804,2.04890939607611,-4.70080124019754));
#30968=CARTESIAN_POINT('Ctrl Pts',(-38.1568684786975,4.05174953100885,-3.14306979737026));
#30969=CARTESIAN_POINT('Ctrl Pts',(-38.0176098346146,5.06260700763802,-0.815826145318977));
#30970=CARTESIAN_POINT('Ctrl Pts',(-37.8783511905319,4.83399538111841,1.71115477631265));
#30971=CARTESIAN_POINT('Ctrl Pts',(-37.7390925464489,3.42188523088942,3.81919670608788));
#30972=CARTESIAN_POINT('Ctrl Pts',(-37.5998339023662,1.17200098288635,4.99219147362009));
#30973=CARTESIAN_POINT('Ctrl Pts',(-37.4605752582833,-1.36482218906556,
4.94295684842645));
#30974=CARTESIAN_POINT('Ctrl Pts',(-37.3213166142005,-3.56749836282337,
3.68354685655336));
#30975=CARTESIAN_POINT('Ctrl Pts',(-37.2004946734363,-4.72076817860514,
1.80843190677617));
#30976=CARTESIAN_POINT('Ctrl Pts',(-37.1260922806997,-4.91763167831984,
0.494150831035411));
#30977=CARTESIAN_POINT('Ctrl Pts',(-37.0981094359907,-4.91789617187166,
-7.46432797522553E-5));
#30978=CARTESIAN_POINT('Origin',(-62.8183905640093,0.,0.));
#30979=CARTESIAN_POINT('',(-40.9433905640093,-4.91845884819695,-0.000108359509173095));
#30980=CARTESIAN_POINT('',(-40.5981094359907,-4.91783128990945,2.3246260680565E-5));
#30981=CARTESIAN_POINT('',(-62.8183905640093,-4.91825,1.40632325245411E-12));
#30982=CARTESIAN_POINT('Ctrl Pts',(-40.9433905640093,-4.91845884819695,
-0.000108359509173109));
#30983=CARTESIAN_POINT('Ctrl Pts',(-40.9364576069728,-4.9185764495009,-0.12251612456806));
#30984=CARTESIAN_POINT('Ctrl Pts',(-40.8831051019086,-4.88412565353057,
-1.06443786785133));
#30985=CARTESIAN_POINT('Ctrl Pts',(-40.7833330488169,-4.30423326894481,
-2.78731735811214));
#30986=CARTESIAN_POINT('Ctrl Pts',(-40.6440744047341,-2.4410402010708,-4.50964353636523));
#30987=CARTESIAN_POINT('Ctrl Pts',(-40.5048157606512,0.0197884139050482,
-5.12788167833459));
#30988=CARTESIAN_POINT('Ctrl Pts',(-40.3655571165684,2.47577226656799,-4.49066963518998));
#30989=CARTESIAN_POINT('Ctrl Pts',(-40.2262984724856,4.32561718207586,-2.75401490236612));
#30990=CARTESIAN_POINT('Ctrl Pts',(-40.0870398284027,5.11642890754077,-0.343099580888201));
#30991=CARTESIAN_POINT('Ctrl Pts',(-39.94778118432,4.65459440947177,2.15181620303378));
#30992=CARTESIAN_POINT('Ctrl Pts',(-39.808522540237,3.0531838096976,4.11990663881172));
#30993=CARTESIAN_POINT('Ctrl Pts',(-39.6692638961543,0.704267627790603,
5.07932763235163));
#30994=CARTESIAN_POINT('Ctrl Pts',(-39.5300052520714,-1.81707314952296,
4.79518584182169));
#30995=CARTESIAN_POINT('Ctrl Pts',(-39.3907466079886,-3.89354312734584,
3.33704719832106));
#30996=CARTESIAN_POINT('Ctrl Pts',(-39.2785417119678,-4.79855598410901,
1.50389656853719));
#30997=CARTESIAN_POINT('Ctrl Pts',(-39.2127563639747,-4.91802127137425,
0.342099902225225));
#30998=CARTESIAN_POINT('Ctrl Pts',(-39.1933905640093,-4.91787152802865,
6.14470143736612E-5));
#30999=CARTESIAN_POINT('Ctrl Pts',(-40.5981094359907,-4.91783128990945,
2.32462606805997E-5));
#31000=CARTESIAN_POINT('Ctrl Pts',(-40.5734947666957,-4.91775999740035,
-0.434730829549026));
#31001=CARTESIAN_POINT('Ctrl Pts',(-40.5024605493732,-4.75302315511206,
-1.68941841504038));
#31002=CARTESIAN_POINT('Ctrl Pts',(-40.3850067840229,-3.69875772681961,
-3.5517253964044));
#31003=CARTESIAN_POINT('Ctrl Pts',(-40.2457481399401,-1.54321132674375,
-4.89020048813763));
#31004=CARTESIAN_POINT('Ctrl Pts',(-40.1064894958572,0.990156768012798,
-5.03141645940088));
#31005=CARTESIAN_POINT('Ctrl Pts',(-39.9672308517744,3.28110653573467,-3.9407996541731));
#31006=CARTESIAN_POINT('Ctrl Pts',(-39.8279722076915,4.76874880416872,-1.88536385239323));
#31007=CARTESIAN_POINT('Ctrl Pts',(-39.6887135636088,5.08886675271635,0.631662240655434));
#31008=CARTESIAN_POINT('Ctrl Pts',(-39.5494549195259,4.16308647125779,2.99403958657897));
#31009=CARTESIAN_POINT('Ctrl Pts',(-39.410196275443,2.21806510569457,4.62339152571701));
#31010=CARTESIAN_POINT('Ctrl Pts',(-39.2709376313602,-0.270001209463393,
5.12080670989053));
#31011=CARTESIAN_POINT('Ctrl Pts',(-39.1316789872773,-2.69196360692879,
4.36450386093798));
#31012=CARTESIAN_POINT('Ctrl Pts',(-38.9924203431946,-4.45485732445219,
2.53964726526075));
#31013=CARTESIAN_POINT('Ctrl Pts',(-38.8978971594323,-4.91113255473073,
0.878970252247324));
#31014=CARTESIAN_POINT('Ctrl Pts',(-38.8497935236977,-4.91867055455711,
0.0297621167608296));
#31015=CARTESIAN_POINT('Ctrl Pts',(-38.8481094359907,-4.91866022846763,
3.15193572706382E-5));
#31016=CARTESIAN_POINT('Origin',(-62.8183905640093,0.,0.));
#31017=CARTESIAN_POINT('',(-42.6933905640093,-4.91811507793926,0.00012467419432587));
#31018=CARTESIAN_POINT('',(-42.3481094359907,-4.91857378612503,-7.83346265964546E-5));
#31019=CARTESIAN_POINT('',(-62.8183905640093,-4.91825,1.40632325245411E-12));
#31020=CARTESIAN_POINT('Ctrl Pts',(-42.6933905640093,-4.91811507793926,
0.000124674194325845));
#31021=CARTESIAN_POINT('Ctrl Pts',(-42.6601588499708,-4.91755631155856,
-0.586730043688538));
#31022=CARTESIAN_POINT('Ctrl Pts',(-42.5805075879047,-4.66566210384887,
-1.99379652867801));
#31023=CARTESIAN_POINT('Ctrl Pts',(-42.454436777811,-3.35365447446679,-3.87924783356431));
#31024=CARTESIAN_POINT('Ctrl Pts',(-42.3151781337281,-1.08333295532153,
-5.01218034354698));
#31025=CARTESIAN_POINT('Ctrl Pts',(-42.1759194896453,1.45221905169649,-4.91798962119831));
#31026=CARTESIAN_POINT('Ctrl Pts',(-42.0366608455625,3.63222684150266,-3.61973621417252));
#31027=CARTESIAN_POINT('Ctrl Pts',(-41.8974022014796,4.9229629697167,-1.43526920371147));
#31028=CARTESIAN_POINT('Ctrl Pts',(-41.7581435573968,5.00841879714827,1.10059222271303));
#31029=CARTESIAN_POINT('Ctrl Pts',(-41.618884913314,3.8676723249881,3.36699760541134));
#31030=CARTESIAN_POINT('Ctrl Pts',(-41.4796262692311,1.78001049070443,4.80906693042493));
#31031=CARTESIAN_POINT('Ctrl Pts',(-41.3403676251483,-0.743448157983408,
5.07374092014123));
#31032=CARTESIAN_POINT('Ctrl Pts',(-41.2011089810654,-3.08488971148233,
4.09621991063895));
#31033=CARTESIAN_POINT('Ctrl Pts',(-41.0687832940191,-4.59209593044371,
2.21442192660095));
#31034=CARTESIAN_POINT('Ctrl Pts',(-40.9828771550004,-4.91778905108657,
0.697063904442349));
#31035=CARTESIAN_POINT('Ctrl Pts',(-40.9433905640093,-4.91845884819695,
-0.000108359509173109));
#31036=CARTESIAN_POINT('Ctrl Pts',(-42.3481094359907,-4.91857378612503,
-7.83346265965153E-5));
#31037=CARTESIAN_POINT('Ctrl Pts',(-42.3436155577213,-4.91863393370315,
-0.0794165444578229));
#31038=CARTESIAN_POINT('Ctrl Pts',(-42.2927021314243,-4.89733658468067,
-0.978247065527181));
#31039=CARTESIAN_POINT('Ctrl Pts',(-42.1953691570999,-4.37596721157521,
-2.67328879404945));
#31040=CARTESIAN_POINT('Ctrl Pts',(-42.0561105130169,-2.5586604085778,-4.44396432554854));
#31041=CARTESIAN_POINT('Ctrl Pts',(-41.9168518689342,-0.114921311488126,
-5.12663194556987));
#31042=CARTESIAN_POINT('Ctrl Pts',(-41.7775932248512,2.35695376666187,-4.55415535033556));
#31043=CARTESIAN_POINT('Ctrl Pts',(-41.6383345807685,4.25178003045199,-2.86669297027451));
#31044=CARTESIAN_POINT('Ctrl Pts',(-41.4990759366856,5.10565052319778,-0.477383229849849));
#31045=CARTESIAN_POINT('Ctrl Pts',(-41.3598172926028,4.70951364514992,2.02880340085441));
#31046=CARTESIAN_POINT('Ctrl Pts',(-41.2205586485199,3.16035488623825,4.03828168980343));
#31047=CARTESIAN_POINT('Ctrl Pts',(-41.0813000044371,0.837452040422802,
5.05907462814725));
#31048=CARTESIAN_POINT('Ctrl Pts',(-40.9420413603542,-1.6904827045519,4.84126328955393));
#31049=CARTESIAN_POINT('Ctrl Pts',(-40.8027827162714,-3.80453956437015,
3.43817403810713));
#31050=CARTESIAN_POINT('Ctrl Pts',(-40.6881387414835,-4.77810753769317,
1.59011154568654));
#31051=CARTESIAN_POINT('Ctrl Pts',(-40.6199143147233,-4.91789444430315,
0.385149683993097));
#31052=CARTESIAN_POINT('Ctrl Pts',(-40.5981094359907,-4.91783128990945,
2.32462606805997E-5));
#31053=CARTESIAN_POINT('Origin',(-62.8183905640093,0.,0.));
#31054=CARTESIAN_POINT('',(-44.4433905640093,-4.91811906887483,-0.000125018227360122));
#31055=CARTESIAN_POINT('',(-44.0981094359908,-4.9179985551391,0.000107459425146145));
#31056=CARTESIAN_POINT('',(-62.8183905640093,-4.91825,1.40632325245411E-12));
#31057=CARTESIAN_POINT('Ctrl Pts',(-44.4433905640092,-4.91811906887483,
-0.000125018227360024));
#31058=CARTESIAN_POINT('Ctrl Pts',(-44.4302796409964,-4.91834041492064,
-0.231656533346569));
#31059=CARTESIAN_POINT('Ctrl Pts',(-44.3707491699559,-4.84545805489063,
-1.2827929143631));
#31060=CARTESIAN_POINT('Ctrl Pts',(-44.2647991508879,-4.10936474789597,
-3.06735773216533));
#31061=CARTESIAN_POINT('Ctrl Pts',(-44.125540506805,-2.13576953418586,-4.66197925619238));
#31062=CARTESIAN_POINT('Ctrl Pts',(-43.9862818627222,0.360722350167653,
-5.11521665957699));
#31063=CARTESIAN_POINT('Ctrl Pts',(-43.8470232186393,2.7688992207005,-4.31610463194866));
#31064=CARTESIAN_POINT('Ctrl Pts',(-43.7077645745566,4.49917140129531,-2.46028835506957));
#31065=CARTESIAN_POINT('Ctrl Pts',(-43.5685059304736,5.12791941987977,-0.00212403965129634));
#31066=CARTESIAN_POINT('Ctrl Pts',(-43.4292472863909,4.50120801315461,2.4565603006312));
#31067=CARTESIAN_POINT('Ctrl Pts',(-43.289988642308,2.77247382434629,4.31380933533684));
#31068=CARTESIAN_POINT('Ctrl Pts',(-43.1507299982252,0.364959781723236,
5.11491607419408));
#31069=CARTESIAN_POINT('Ctrl Pts',(-43.0114713541423,-2.13190671757982,
4.66374697382507));
#31070=CARTESIAN_POINT('Ctrl Pts',(-42.8722127100594,-4.10682227278453,
3.0707609656379));
#31071=CARTESIAN_POINT('Ctrl Pts',(-42.7661857800152,-4.84492911504421,
1.28551155191592));
#31072=CARTESIAN_POINT('Ctrl Pts',(-42.7065783979984,-4.91833682148999,
0.233014936376255));
#31073=CARTESIAN_POINT('Ctrl Pts',(-42.6933905640093,-4.91811507793926,
0.000124674194325845));
#31074=CARTESIAN_POINT('Ctrl Pts',(-44.0981094359908,-4.9179985551391,0.000107459425145867));
#31075=CARTESIAN_POINT('Ctrl Pts',(-44.0673168007194,-4.91756779448751,
-0.543711354100132));
#31076=CARTESIAN_POINT('Ctrl Pts',(-43.9901046174204,-4.69201025116029,
-1.90767934972549));
#31077=CARTESIAN_POINT('Ctrl Pts',(-43.8664728860938,-3.45440006425625,
-3.78981295174814));
#31078=CARTESIAN_POINT('Ctrl Pts',(-43.7272142420111,-1.21462268519213,
-4.98199294919094));
#31079=CARTESIAN_POINT('Ctrl Pts',(-43.5879555979281,1.32252861367418,-4.95444044057296));
#31080=CARTESIAN_POINT('Ctrl Pts',(-43.4486969538454,3.53588757546868,-3.71390105775826));
#31081=CARTESIAN_POINT('Ctrl Pts',(-43.3094383097624,4.88356144746871,-1.56409385970568));
#31082=CARTESIAN_POINT('Ctrl Pts',(-43.1701796656797,5.03560162356189,0.968647666570477));
#31083=CARTESIAN_POINT('Ctrl Pts',(-43.0309210215968,3.95478437683829,3.26423690100571));
#31084=CARTESIAN_POINT('Ctrl Pts',(-42.891662377514,1.90572427869227,4.76064879893219));
#31085=CARTESIAN_POINT('Ctrl Pts',(-42.7524037334311,-0.60991091781632,
5.09151948690174));
#31086=CARTESIAN_POINT('Ctrl Pts',(-42.6131450893483,-2.97622270502889,
4.17584248065492));
#31087=CARTESIAN_POINT('Ctrl Pts',(-42.4783803235348,-4.56102422386236,
2.30034197151273));
#31088=CARTESIAN_POINT('Ctrl Pts',(-42.3900351057489,-4.91801263886073,
0.740108066787903));
#31089=CARTESIAN_POINT('Ctrl Pts',(-42.3481094359907,-4.91857378612503,
-7.83346265965153E-5));
#31090=CARTESIAN_POINT('Origin',(-62.8183905640093,0.,0.));
#31091=CARTESIAN_POINT('',(-46.1933905640093,-4.91845483554336,0.000109107315461253));
#31092=CARTESIAN_POINT('',(-45.8481094359907,-4.91825200889249,-0.000129049404935799));
#31093=CARTESIAN_POINT('',(-62.8183905640093,-4.91825,1.40632325245411E-12));
#31094=CARTESIAN_POINT('Ctrl Pts',(-46.1933905640093,-4.91845483554336,
0.000109107315461165));
#31095=CARTESIAN_POINT('Ctrl Pts',(-46.1539808839944,-4.91778337373426,
-0.695706862165678));
#31096=CARTESIAN_POINT('Ctrl Pts',(-46.068151655952,-4.59305371007858,-2.21171144892918));
#31097=CARTESIAN_POINT('Ctrl Pts',(-45.9359028798819,-3.0882820494734,-4.09366291616992));
#31098=CARTESIAN_POINT('Ctrl Pts',(-45.7966442357991,-0.747651098816729,
-5.07312329071181));
#31099=CARTESIAN_POINT('Ctrl Pts',(-45.6573855917162,1.77602594558582,-4.81053987915395));
#31100=CARTESIAN_POINT('Ctrl Pts',(-45.5181269476334,3.86488170470528,-3.37020051287143));
#31101=CARTESIAN_POINT('Ctrl Pts',(-45.3788683035506,5.00750532432036,-1.10474092674605));
#31102=CARTESIAN_POINT('Ctrl Pts',(-45.2396096594678,4.92415028827758,1.43119042296277));
#31103=CARTESIAN_POINT('Ctrl Pts',(-45.1003510153849,3.63522426235287,3.61672595737161));
#31104=CARTESIAN_POINT('Ctrl Pts',(-44.9610923713021,1.45629272160045,4.91678488418377));
#31105=CARTESIAN_POINT('Ctrl Pts',(-44.8218337272192,-1.07918038574816,
5.01307607994741));
#31106=CARTESIAN_POINT('Ctrl Pts',(-44.6825750831364,-3.35043967147466,
3.88202474182395));
#31107=CARTESIAN_POINT('Ctrl Pts',(-44.5564273620664,-4.66481015725751,
1.99651140099669));
#31108=CARTESIAN_POINT('Ctrl Pts',(-44.476699189024,-4.91755673375692,0.588086537026348));
#31109=CARTESIAN_POINT('Ctrl Pts',(-44.4433905640092,-4.91811906887483,
-0.000125018227360024));
#31110=CARTESIAN_POINT('Ctrl Pts',(-45.8481094359907,-4.91825200889249,
-0.000129049404935973));
#31111=CARTESIAN_POINT('Ctrl Pts',(-45.837437591745,-4.91844704284713,-0.18857316690703));
#31112=CARTESIAN_POINT('Ctrl Pts',(-45.7803461994717,-4.86162270123637,
-1.19657974072127));
#31113=CARTESIAN_POINT('Ctrl Pts',(-45.6768352591708,-4.1885222391554,-2.95835147764295));
#31114=CARTESIAN_POINT('Ctrl Pts',(-45.5375766150878,-2.25749675029642,
-4.60426654697279));
#31115=CARTESIAN_POINT('Ctrl Pts',(-45.3983179710051,0.226227667835505,
-5.12292719599619));
#31116=CARTESIAN_POINT('Ctrl Pts',(-45.2590593269221,2.65456516690845,-4.38735065703757));
#31117=CARTESIAN_POINT('Ctrl Pts',(-45.1198006828394,4.43299017984253,-2.57762683074788));
#31118=CARTESIAN_POINT('Ctrl Pts',(-44.9805420387565,5.12609406194675,-0.136827194832999));
#31119=CARTESIAN_POINT('Ctrl Pts',(-44.8412833946737,4.56418541788972,2.33747160074608));
#31120=CARTESIAN_POINT('Ctrl Pts',(-44.7020247505909,2.88483534533912,4.23949136612563));
#31121=CARTESIAN_POINT('Ctrl Pts',(-44.562766106508,0.499196146884659,5.10356397237334));
#31122=CARTESIAN_POINT('Ctrl Pts',(-44.4235074624252,-2.00866035967626,
4.71814005436855));
#31123=CARTESIAN_POINT('Ctrl Pts',(-44.2842488183423,-4.02474010956177,
3.17758226701629));
#31124=CARTESIAN_POINT('Ctrl Pts',(-44.1757828095309,-4.82754107525667,
1.37172977179825));
#31125=CARTESIAN_POINT('Ctrl Pts',(-44.113736348747,-4.91821716127859,0.276089332340098));
#31126=CARTESIAN_POINT('Ctrl Pts',(-44.0981094359908,-4.9179985551391,0.000107459425145867));
#31127=CARTESIAN_POINT('Origin',(-62.8183905640093,0.,0.));
#31128=CARTESIAN_POINT('',(-47.9433905640093,-4.91787338031339,-6.25745746822065E-5));
#31129=CARTESIAN_POINT('',(-47.5981094359907,-4.91832100844767,0.000125872292329049));
#31130=CARTESIAN_POINT('',(-62.8183905640093,-4.91825,1.40632325245411E-12));
#31131=CARTESIAN_POINT('Ctrl Pts',(-47.9433905640093,-4.91787338031339,
-6.25745746826376E-5));
#31132=CARTESIAN_POINT('Ctrl Pts',(-47.9241016750201,-4.918025336644,-0.34074226218686));
#31133=CARTESIAN_POINT('Ctrl Pts',(-47.8583932380032,-4.79918089678194,
-1.50117787435966));
#31134=CARTESIAN_POINT('Ctrl Pts',(-47.7462652529588,-3.89630627287599,
-3.33382055849918));
#31135=CARTESIAN_POINT('Ctrl Pts',(-47.607006608876,-1.82104496094234,-4.79367889397601));
#31136=CARTESIAN_POINT('Ctrl Pts',(-47.4677479647931,0.700059562034036,
-5.07990931985298));
#31137=CARTESIAN_POINT('Ctrl Pts',(-47.3284893207103,3.04976974288669,-4.12243454813989));
#31138=CARTESIAN_POINT('Ctrl Pts',(-47.1892306766275,4.65281020153438,-2.15567143062717));
#31139=CARTESIAN_POINT('Ctrl Pts',(-47.0499720325446,5.11671138294472,0.33886090357014));
#31140=CARTESIAN_POINT('Ctrl Pts',(-46.9107133884618,4.32789718286852,2.75043052318056));
#31141=CARTESIAN_POINT('Ctrl Pts',(-46.771454744379,2.47949158419529,4.48861711134167));
#31142=CARTESIAN_POINT('Ctrl Pts',(-46.6321961002961,0.0240364544226033,
5.12786352560043));
#31143=CARTESIAN_POINT('Ctrl Pts',(-46.4929374562133,-2.43730347789571,
4.51166419904695));
#31144=CARTESIAN_POINT('Ctrl Pts',(-46.3536788121304,-4.30192271842598,
2.79088212094582));
#31145=CARTESIAN_POINT('Ctrl Pts',(-46.2538298480624,-4.88369029434119,
1.06715587713395));
#31146=CARTESIAN_POINT('Ctrl Pts',(-46.2004004320221,-4.91857426961782,
0.123875098447742));
#31147=CARTESIAN_POINT('Ctrl Pts',(-46.1933905640093,-4.91845483554336,
0.000109107315461165));
#31148=CARTESIAN_POINT('Ctrl Pts',(-47.5981094359907,-4.91832100844767,
0.000125872292329066));
#31149=CARTESIAN_POINT('Ctrl Pts',(-47.561138834743,-4.91764271032085,-0.652677035677827));
#31150=CARTESIAN_POINT('Ctrl Pts',(-47.4777486854677,-4.62273622332759,
-2.1257206615366));
#31151=CARTESIAN_POINT('Ctrl Pts',(-47.3479389881648,-3.1947516251322,-4.01112503755328));
#31152=CARTESIAN_POINT('Ctrl Pts',(-47.2086803440819,-0.880657560390307,
-5.05173279919862));
#31153=CARTESIAN_POINT('Ctrl Pts',(-47.0694216999991,1.6490463344078,-4.85553377087915));
#31154=CARTESIAN_POINT('Ctrl Pts',(-46.9301630559163,3.7750171371299,-3.47056301304949));
#31155=CARTESIAN_POINT('Ctrl Pts',(-46.7909044118334,4.97675718319434,-1.23590046229263));
#31156=CARTESIAN_POINT('Ctrl Pts',(-46.6516457677506,4.96004658650958,1.30134540873142));
#31157=CARTESIAN_POINT('Ctrl Pts',(-46.5123871236678,3.72897657285209,3.51998518921485));
#31158=CARTESIAN_POINT('Ctrl Pts',(-46.3731284795849,1.58494783230892,4.87683323295259));
#31159=CARTESIAN_POINT('Ctrl Pts',(-46.2338698355021,-0.947120877618752,
5.03969483762166));
#31160=CARTESIAN_POINT('Ctrl Pts',(-46.0946111914193,-3.24730766130082,
3.9686968851285));
#31161=CARTESIAN_POINT('Ctrl Pts',(-45.9660243915821,-4.63711698689941,
2.08258460884));
#31162=CARTESIAN_POINT('Ctrl Pts',(-45.8838571397726,-4.91759869950401,
0.631106221350268));
#31163=CARTESIAN_POINT('Ctrl Pts',(-45.8481094359907,-4.91825200889249,
-0.000129049404935973));
#31164=CARTESIAN_POINT('Origin',(-62.8183905640093,0.,0.));
#31165=CARTESIAN_POINT('',(-49.6933905640093,-4.91867246230615,1.57158398012151E-5));
#31166=CARTESIAN_POINT('',(-49.3481094359907,-4.91794918791349,-9.46638502663522E-5));
#31167=CARTESIAN_POINT('',(-62.8183905640093,-4.91825,1.40632325245411E-12));
#31168=CARTESIAN_POINT('Ctrl Pts',(-49.6933905640093,-4.91867246230615,
1.57158398011309E-5));
#31169=CARTESIAN_POINT('Ctrl Pts',(-49.6478029180181,-4.91852637123773,
-0.804774992398663));
#31170=CARTESIAN_POINT('Ctrl Pts',(-49.5557957239992,-4.51180610137747,
-2.4291848203257));
#31171=CARTESIAN_POINT('Ctrl Pts',(-49.4173689819529,-2.80923945602917,
-4.28995754839293));
#31172=CARTESIAN_POINT('Ctrl Pts',(-49.27811033787,-0.408659791847362,-5.11161024168038));
#31173=CARTESIAN_POINT('Ctrl Pts',(-49.1388516937872,2.09197132506023,-4.68179645685823));
#31174=CARTESIAN_POINT('Ctrl Pts',(-48.9995930497043,4.08042880925776,-3.10574674126912));
#31175=CARTESIAN_POINT('Ctrl Pts',(-48.8603344056215,5.06988213827541,-0.769322554147787));
#31176=CARTESIAN_POINT('Ctrl Pts',(-48.7210757615387,4.81808520680125,1.75545351072806));
#31177=CARTESIAN_POINT('Ctrl Pts',(-48.5818171174558,3.38668501140426,3.85044500309434));
#31178=CARTESIAN_POINT('Ctrl Pts',(-48.442558473373,1.12612872559781,5.00273886803099));
#31179=CARTESIAN_POINT('Ctrl Pts',(-48.3032998292901,-1.4101356606875,4.93022104035731));
#31180=CARTESIAN_POINT('Ctrl Pts',(-48.1640411852073,-3.60115903181333,
3.65064593132692));
#31181=CARTESIAN_POINT('Ctrl Pts',(-48.0440714301137,-4.72915620559369,
1.77832394507212));
#31182=CARTESIAN_POINT('Ctrl Pts',(-47.9705212230477,-4.91765964714312,
0.479118183377995));
#31183=CARTESIAN_POINT('Ctrl Pts',(-47.9433905640093,-4.91787338031339,
-6.25745746826376E-5));
#31184=CARTESIAN_POINT('Ctrl Pts',(-49.3481094359907,-4.91794918791349,
-9.46638502663175E-5));
#31185=CARTESIAN_POINT('Ctrl Pts',(-49.3312596257687,-4.918154011868,-0.297682293376429));
#31186=CARTESIAN_POINT('Ctrl Pts',(-49.267990267519,-4.81837287639424,-1.41495845453493));
#31187=CARTESIAN_POINT('Ctrl Pts',(-49.1583013612416,-3.98253692500126,
-3.23031912574798));
#31188=CARTESIAN_POINT('Ctrl Pts',(-49.0190427171589,-1.94634036455058,
-4.74418814956709));
#31189=CARTESIAN_POINT('Ctrl Pts',(-48.879784073076,0.566375258594887,-5.09654599504637));
#31190=CARTESIAN_POINT('Ctrl Pts',(-48.7405254289932,2.94042623074984,-4.20112551522683));
#31191=CARTESIAN_POINT('Ctrl Pts',(-48.6012667849103,4.5945778590284,-2.27715091956982));
#31192=CARTESIAN_POINT('Ctrl Pts',(-48.4620081408275,5.12384713130236,0.20433450079776));
#31193=CARTESIAN_POINT('Ctrl Pts',(-48.3227494967446,4.39865398946333,2.63579306739927));
#31194=CARTESIAN_POINT('Ctrl Pts',(-48.1834908526618,2.59654618544401,4.42193508772209));
#31195=CARTESIAN_POINT('Ctrl Pts',(-48.0442322085789,0.158730579712837,
5.12546257583017));
#31196=CARTESIAN_POINT('Ctrl Pts',(-47.9049735644962,-2.31794675259165,
4.57413214340397));
#31197=CARTESIAN_POINT('Ctrl Pts',(-47.7657149204133,-4.22712528867379,
2.90292504330135));
#31198=CARTESIAN_POINT('Ctrl Pts',(-47.6634268775782,-4.86928460793813,
1.15335712439825));
#31199=CARTESIAN_POINT('Ctrl Pts',(-47.6075583827706,-4.91849436789233,
0.166969248569943));
#31200=CARTESIAN_POINT('Ctrl Pts',(-47.5981094359907,-4.91832100844767,
0.000125872292329066));
#31201=CARTESIAN_POINT('Origin',(-62.8183905640093,0.,0.));
#31202=CARTESIAN_POINT('',(-51.4433905640093,-4.91784119574401,3.70365089225223E-5));
#31203=CARTESIAN_POINT('',(-51.0981094359907,-4.91861900665162,5.92428380992091E-5));
#31204=CARTESIAN_POINT('',(-62.8183905640093,-4.91825,1.40632325245411E-12));
#31205=CARTESIAN_POINT('Ctrl Pts',(-51.4433905640093,-4.91784119574402,
3.70365089222974E-5));
#31206=CARTESIAN_POINT('Ctrl Pts',(-51.4179237090437,-4.91772339455084,
-0.449766092710603));
#31207=CARTESIAN_POINT('Ctrl Pts',(-51.3460373060505,-4.74508883257368,
-1.71953364257664));
#31208=CARTESIAN_POINT('Ctrl Pts',(-51.2277313550298,-3.66600093949493,
-3.58552634907998));
#31209=CARTESIAN_POINT('Ctrl Pts',(-51.0884727109469,-1.49825959824569,
-4.90415948604745));
#31210=CARTESIAN_POINT('Ctrl Pts',(-50.9492140668641,1.03629798564688,-5.02211594582091));
#31211=CARTESIAN_POINT('Ctrl Pts',(-50.8099554227812,3.31714056994997,-3.91051665736339));
#31212=CARTESIAN_POINT('Ctrl Pts',(-50.6706967786984,4.78585350621771,-1.84151250480363));
#31213=CARTESIAN_POINT('Ctrl Pts',(-50.5314381346155,5.08285440870451,0.678345891295609));
#31214=CARTESIAN_POINT('Ctrl Pts',(-50.3921794905327,4.13542907271616,3.03212606480312));
#31215=CARTESIAN_POINT('Ctrl Pts',(-50.2529208464499,2.17553396450143,4.64355618654767));
#31216=CARTESIAN_POINT('Ctrl Pts',(-50.113662202367,-0.316993269371489,
5.11811267514673));
#31217=CARTESIAN_POINT('Ctrl Pts',(-49.9744035582842,-2.73191160279071,
4.33961070637241));
#31218=CARTESIAN_POINT('Ctrl Pts',(-49.8351449142014,-4.47798085922564,
2.49864953779702));
#31219=CARTESIAN_POINT('Ctrl Pts',(-49.7414739161098,-4.91501765406269,
0.848863542292382));
#31220=CARTESIAN_POINT('Ctrl Pts',(-49.6942224660457,-4.91867512823581,
0.0147018663202137));
#31221=CARTESIAN_POINT('Ctrl Pts',(-49.6933905640093,-4.91867246230615,
1.57158398011309E-5));
#31222=CARTESIAN_POINT('Ctrl Pts',(-51.0981094359907,-4.91861900665162,
5.92428380991137E-5));
#31223=CARTESIAN_POINT('Ctrl Pts',(-51.0549608687667,-4.91815886707571,
-0.761696767512525));
#31224=CARTESIAN_POINT('Ctrl Pts',(-50.965392753515,-4.54493313080541,-2.3433907057031));
#31225=CARTESIAN_POINT('Ctrl Pts',(-50.8294050902357,-2.92096173384329,
-4.21468202390108));
#31226=CARTESIAN_POINT('Ctrl Pts',(-50.6901464461529,-0.542794236847172,
-5.09911133724467));
#31227=CARTESIAN_POINT('Ctrl Pts',(-50.55088780207,1.96826461136862,-4.73513425710461));
#31228=CARTESIAN_POINT('Ctrl Pts',(-50.4116291579872,3.99743672238916,-3.21186264707355));
#31229=CARTESIAN_POINT('Ctrl Pts',(-50.2723705139044,5.04792348380256,-0.902236396320984));
#31230=CARTESIAN_POINT('Ctrl Pts',(-50.1331118698215,4.86253608318979,1.62828279265274));
#31231=CARTESIAN_POINT('Ctrl Pts',(-49.9938532257387,3.48666258935134,3.76015239068703));
#31232=CARTESIAN_POINT('Ctrl Pts',(-49.8545945816558,1.25715567184686,4.97143054159615));
#31233=CARTESIAN_POINT('Ctrl Pts',(-49.7153359375731,-1.28013844121747,
4.96556216198015));
#31234=CARTESIAN_POINT('Ctrl Pts',(-49.5760772934901,-3.50401852802057,
3.74398399682213));
#31235=CARTESIAN_POINT('Ctrl Pts',(-49.4536684596294,-4.70473504165732,
1.86448895312075));
#31236=CARTESIAN_POINT('Ctrl Pts',(-49.3776791737963,-4.91758974228464,
0.52214197046708));
#31237=CARTESIAN_POINT('Ctrl Pts',(-49.3481094359907,-4.91794918791349,
-9.46638502663175E-5));
#31238=CARTESIAN_POINT('Origin',(-62.8183905640093,0.,0.));
#31239=CARTESIAN_POINT('',(-53.1933905640093,-4.91853679395484,-9.01493930066358E-5));
#31240=CARTESIAN_POINT('',(-52.8481094359907,-4.91782510432338,-3.02706344698644E-6));
#31241=CARTESIAN_POINT('',(-62.8183905640093,-4.91825,1.40632325245411E-12));
#31242=CARTESIAN_POINT('Ctrl Pts',(-53.1933905640093,-4.91853679395484,
-9.01493930066492E-5));
#31243=CARTESIAN_POINT('Ctrl Pts',(-53.1880445000694,-4.9186164742464,-0.0944755243151697));
#31244=CARTESIAN_POINT('Ctrl Pts',(-53.1362788881018,-4.8928518455894,-1.00835989416069));
#31245=CARTESIAN_POINT('Ctrl Pts',(-53.0380937281066,-4.35124498857135,
-2.71334279768651));
#31246=CARTESIAN_POINT('Ctrl Pts',(-52.8988350840238,-2.51776186605044,
-4.46726283916524));
#31247=CARTESIAN_POINT('Ctrl Pts',(-52.759576439941,-0.0678595671353494,
-5.12747083536052));
#31248=CARTESIAN_POINT('Ctrl Pts',(-52.6203177958581,2.39865666935982,-4.53232923239918));
#31249=CARTESIAN_POINT('Ctrl Pts',(-52.4810591517753,4.27791404372175,-2.82754549439134));
#31250=CARTESIAN_POINT('Ctrl Pts',(-52.3418005076925,5.10981730287787,-0.430498803174167));
#31251=CARTESIAN_POINT('Ctrl Pts',(-52.2025418636096,4.69069304595447,2.07194614721496));
#31252=CARTESIAN_POINT('Ctrl Pts',(-52.0632832195268,3.12315472211971,4.06712019370289));
#31253=CARTESIAN_POINT('Ctrl Pts',(-51.924024575444,0.790979961646617,5.06654840977544));
#31254=CARTESIAN_POINT('Ctrl Pts',(-51.7847659313611,-1.73484902128376,
4.82554255619773));
#31255=CARTESIAN_POINT('Ctrl Pts',(-51.6455072872782,-3.83593799234573,
3.40310766905826));
#31256=CARTESIAN_POINT('Ctrl Pts',(-51.531715498161,-4.78539130338917,1.55998982552279));
#31257=CARTESIAN_POINT('Ctrl Pts',(-51.4643432570714,-4.91793811592698,
0.370109702239623));
#31258=CARTESIAN_POINT('Ctrl Pts',(-51.4433905640093,-4.91784119574402,
3.70365089222974E-5));
#31259=CARTESIAN_POINT('Ctrl Pts',(-52.8481094359907,-4.91782510432338,
-3.02706344702114E-6));
#31260=CARTESIAN_POINT('Ctrl Pts',(-52.8250816597923,-4.91783377634347,
-0.406730229006752));
#31261=CARTESIAN_POINT('Ctrl Pts',(-52.7556343355662,-4.76739234533979,
-1.63333459135314));
#31262=CARTESIAN_POINT('Ctrl Pts',(-52.6397674633126,-3.75892305563278,
-3.48798788343709));
#31263=CARTESIAN_POINT('Ctrl Pts',(-52.5005088192298,-1.62656857379318,
-4.86310977543383));
#31264=CARTESIAN_POINT('Ctrl Pts',(-52.3612501751469,0.904015809819905,
-5.04760511814933));
#31265=CARTESIAN_POINT('Ctrl Pts',(-52.2219915310641,3.21327160455789,-3.99630424373741));
#31266=CARTESIAN_POINT('Ctrl Pts',(-52.0827328869813,4.73582780601003,-1.96659528245999));
#31267=CARTESIAN_POINT('Ctrl Pts',(-51.9434742428983,5.09891967722156,0.544591717173908));
#31268=CARTESIAN_POINT('Ctrl Pts',(-51.8042155988156,4.21365207873328,2.92244729166469));
#31269=CARTESIAN_POINT('Ctrl Pts',(-51.6649569547327,2.29676350806032,4.58480527407807));
#31270=CARTESIAN_POINT('Ctrl Pts',(-51.5256983106499,-0.182437602611408,
5.12467350514402));
#31271=CARTESIAN_POINT('Ctrl Pts',(-51.3864396665671,-2.6169728383005,4.40987700245359));
#31272=CARTESIAN_POINT('Ctrl Pts',(-51.2471810224842,-4.41079925105322,
2.61541812719877));
#31273=CARTESIAN_POINT('Ctrl Pts',(-51.1510709456254,-4.90352744261773,
0.935037184879213));
#31274=CARTESIAN_POINT('Ctrl Pts',(-51.1013804167943,-4.91865388863766,
0.0578059873339447));
#31275=CARTESIAN_POINT('Ctrl Pts',(-51.0981094359907,-4.91861900665162,
5.92428380991137E-5));
#31276=CARTESIAN_POINT('Origin',(-62.8183905640093,0.,0.));
#31277=CARTESIAN_POINT('',(-54.9433905640093,-4.91803681242707,0.00011480967905517));
#31278=CARTESIAN_POINT('',(-54.5981094359907,-4.91863036579189,-5.31391465866116E-5));
#31279=CARTESIAN_POINT('',(-62.8183905640093,-4.91825,1.40632325245411E-12));
#31280=CARTESIAN_POINT('Ctrl Pts',(-54.9433905640093,-4.91803681242707,
0.000114809679055));
#31281=CARTESIAN_POINT('Ctrl Pts',(-54.9117457430674,-4.91755857232653,
-0.558741720734804));
#31282=CARTESIAN_POINT('Ctrl Pts',(-54.8336813740978,-4.68295166729167,
-1.93777195873213));
#31283=CARTESIAN_POINT('Ctrl Pts',(-54.7091974571006,-3.41946818595568,
-3.82136093735749));
#31284=CARTESIAN_POINT('Ctrl Pts',(-54.5699388130178,-1.16884224379346,
-4.99293199407404));
#31285=CARTESIAN_POINT('Ctrl Pts',(-54.430680168935,1.36794927382256,-4.94209235775424));
#31286=CARTESIAN_POINT('Ctrl Pts',(-54.2914215248522,3.56982819462436,-3.68128900647443));
#31287=CARTESIAN_POINT('Ctrl Pts',(-54.1521628807693,4.89771240398387,-1.51920219068664));
#31288=CARTESIAN_POINT('Ctrl Pts',(-54.0129042366865,5.02649836382728,1.01482820554322));
#31289=CARTESIAN_POINT('Ctrl Pts',(-53.8736455926037,3.9246556358045,3.30040001040366));
#31290=CARTESIAN_POINT('Ctrl Pts',(-53.7343869485209,1.86194642264088,4.77794072875955));
#31291=CARTESIAN_POINT('Ctrl Pts',(-53.5951283044379,-0.656619833959052,
5.08570668461877));
#31292=CARTESIAN_POINT('Ctrl Pts',(-53.4558696603552,-3.01442702008815,
4.14834808434477));
#31293=CARTESIAN_POINT('Ctrl Pts',(-53.3219570802122,-4.57203450537693,
2.27033105204216));
#31294=CARTESIAN_POINT('Ctrl Pts',(-53.234464048097,-4.91792461512111,0.725066945346297));
#31295=CARTESIAN_POINT('Ctrl Pts',(-53.1933905640093,-4.91853679395484,
-9.01493930066492E-5));
#31296=CARTESIAN_POINT('Ctrl Pts',(-54.5981094359907,-4.91863036579189,
-5.31391465869498E-5));
#31297=CARTESIAN_POINT('Ctrl Pts',(-54.5952024508179,-4.91865864175323,
-0.0513734660281668));
#31298=CARTESIAN_POINT('Ctrl Pts',(-54.5458759176175,-4.90531457595336,
-0.922176319021297));
#31299=CARTESIAN_POINT('Ctrl Pts',(-54.4501298363895,-4.42101949107612,
-2.59810482326958));
#31300=CARTESIAN_POINT('Ctrl Pts',(-54.3108711923067,-2.6342423114104,-4.39958287317637));
#31301=CARTESIAN_POINT('Ctrl Pts',(-54.1716125482239,-0.202528254306939,
-5.12391884394933));
#31302=CARTESIAN_POINT('Ctrl Pts',(-54.0323539041409,2.27877043643476,-4.59377484332902));
#31303=CARTESIAN_POINT('Ctrl Pts',(-53.8930952600582,4.20216179902152,-2.93894508761492));
#31304=CARTESIAN_POINT('Ctrl Pts',(-53.7538366159752,5.09674533424557,-0.564578613673673));
#31305=CARTESIAN_POINT('Ctrl Pts',(-53.6145779718925,4.74350174030785,1.94801264186554));
#31306=CARTESIAN_POINT('Ctrl Pts',(-53.4753193278096,3.22891502039301,3.98367541401808));
#31307=CARTESIAN_POINT('Ctrl Pts',(-53.3360606837268,0.923798757412272,
5.04402199330804));
#31308=CARTESIAN_POINT('Ctrl Pts',(-53.196802039644,-1.60748951844882,4.86944960557646));
#31309=CARTESIAN_POINT('Ctrl Pts',(-53.0575433955611,-3.74521898384984,
3.50269849918351));
#31310=CARTESIAN_POINT('Ctrl Pts',(-52.9413125276768,-4.76414289396322,
1.64619939207857));
#31311=CARTESIAN_POINT('Ctrl Pts',(-52.8715012078199,-4.91781629522634,
0.413153233558466));
#31312=CARTESIAN_POINT('Ctrl Pts',(-52.8481094359907,-4.91782510432338,
-3.02706344702114E-6));
#31313=CARTESIAN_POINT('Origin',(-62.8183905640093,0.,0.));
#31314=CARTESIAN_POINT('',(-56.6933905640093,-4.9182044571118,-0.000129187542790386));
#31315=CARTESIAN_POINT('',(-56.3481094359908,-4.91793587170447,9.03881743496981E-5));
#31316=CARTESIAN_POINT('',(-62.8183905640093,-4.91825,1.40632325245411E-12));
#31317=CARTESIAN_POINT('Ctrl Pts',(-56.6933905640093,-4.9182044571118,-0.000129187542790513));
#31318=CARTESIAN_POINT('Ctrl Pts',(-56.681866534093,-4.91841151819362,-0.203626914331993));
#31319=CARTESIAN_POINT('Ctrl Pts',(-56.623922956149,-4.85610900923186,-1.22670088899472));
#31320=CARTESIAN_POINT('Ctrl Pts',(-56.5195598301776,-4.1611913471364,-2.99667293168903));
#31321=CARTESIAN_POINT('Ctrl Pts',(-56.3803011860948,-2.21513949450856,
-4.62479395317148));
#31322=CARTESIAN_POINT('Ctrl Pts',(-56.2410425420119,0.273241035485556,
-5.12063486534734));
#31323=CARTESIAN_POINT('Ctrl Pts',(-56.1017838979291,2.69472444693603,-4.36279981705527));
#31324=CARTESIAN_POINT('Ctrl Pts',(-55.9625252538462,4.45646324687071,-2.53682821994801));
#31325=CARTESIAN_POINT('Ctrl Pts',(-55.8232666097634,5.1271340465709,-0.089769464874975));
#31326=CARTESIAN_POINT('Ctrl Pts',(-55.6840079656806,4.54253770251526,2.37926738925458));
#31327=CARTESIAN_POINT('Ctrl Pts',(-55.5447493215977,2.84579990176412,4.26579242432466));
#31328=CARTESIAN_POINT('Ctrl Pts',(-55.4054906775149,0.452329953591429,
5.1079310587967));
#31329=CARTESIAN_POINT('Ctrl Pts',(-55.266232033432,-2.05188313562661,4.69950398298055));
#31330=CARTESIAN_POINT('Ctrl Pts',(-55.1269733893492,-4.0537373125207,3.14050567415567));
#31331=CARTESIAN_POINT('Ctrl Pts',(-55.0193595662083,-4.83375182313205,
1.34160576371217));
#31332=CARTESIAN_POINT('Ctrl Pts',(-54.958165291095,-4.91826009910578,0.261040688579662));
#31333=CARTESIAN_POINT('Ctrl Pts',(-54.9433905640093,-4.91803681242707,
0.000114809679055));
#31334=CARTESIAN_POINT('Ctrl Pts',(-56.3481094359908,-4.91793587170447,
9.03881743493859E-5));
#31335=CARTESIAN_POINT('Ctrl Pts',(-56.318903693816,-4.91759809637477,-0.515721651436775));
#31336=CARTESIAN_POINT('Ctrl Pts',(-56.2432784036135,-4.70846037346048,
-1.85163183427517));
#31337=CARTESIAN_POINT('Ctrl Pts',(-56.1212335653836,-3.51867044972994,
-3.73021718930019));
#31338=CARTESIAN_POINT('Ctrl Pts',(-55.9819749213007,-1.29959683625502,
-4.96050502231166));
#31339=CARTESIAN_POINT('Ctrl Pts',(-55.8427162772179,1.23765476786001,-4.97632120032051));
#31340=CARTESIAN_POINT('Ctrl Pts',(-55.7034576331351,3.471893548184,-3.77379347649709));
#31341=CARTESIAN_POINT('Ctrl Pts',(-55.5641989890522,4.85611478302155,-1.64733458267922));
#31342=CARTESIAN_POINT('Ctrl Pts',(-55.4249403449694,5.0514220401755,0.882438318071356));
#31343=CARTESIAN_POINT('Ctrl Pts',(-55.2856817008865,4.00999858994569,3.19616540901837));
#31344=CARTESIAN_POINT('Ctrl Pts',(-55.1464230568037,1.98681429033347,4.72738098622251));
#31345=CARTESIAN_POINT('Ctrl Pts',(-55.0071644127208,-0.522798231506428,
5.10120025310764));
#31346=CARTESIAN_POINT('Ctrl Pts',(-54.867905768638,-2.90441498868291,4.22610170093973));
#31347=CARTESIAN_POINT('Ctrl Pts',(-54.731554109728,-4.54007704180687,2.35620001996191));
#31348=CARTESIAN_POINT('Ctrl Pts',(-54.6416219988456,-4.9182071233356,0.768123792081326));
#31349=CARTESIAN_POINT('Ctrl Pts',(-54.5981094359907,-4.91863036579189,
-5.31391465869498E-5));
#31350=CARTESIAN_POINT('Origin',(-62.8183905640093,0.,0.));
#31351=CARTESIAN_POINT('',(-58.4433905640093,-4.91836886135133,0.000122455552848294));
#31352=CARTESIAN_POINT('',(-58.0981094359908,-4.91834149996792,-0.000124244451389921));
#31353=CARTESIAN_POINT('',(-62.8183905640093,-4.91825,1.40632325245411E-12));
#31354=CARTESIAN_POINT('Ctrl Pts',(-58.4433905640093,-4.91836886135133,
0.000122455552848399));
#31355=CARTESIAN_POINT('Ctrl Pts',(-58.405567777091,-4.91768352809557,-0.667709083104306));
#31356=CARTESIAN_POINT('Ctrl Pts',(-58.321325442145,-4.61251739126612,-2.1557731884816));
#31357=CARTESIAN_POINT('Ctrl Pts',(-58.1906635591718,-3.15779931679017,
-4.04027968761638));
#31358=CARTESIAN_POINT('Ctrl Pts',(-58.0514049150887,-0.834251032978302,
-5.05960384006236));
#31359=CARTESIAN_POINT('Ctrl Pts',(-57.9121462710061,1.69354537464531,-4.84019258737259));
#31360=CARTESIAN_POINT('Ctrl Pts',(-57.772887626923,3.8067141091864,-3.43576636062821));
#31361=CARTESIAN_POINT('Ctrl Pts',(-57.6336289828404,4.98789175297897,-1.19016713333119));
#31362=CARTESIAN_POINT('Ctrl Pts',(-57.4943703387573,4.94789270758304,1.34681839400263));
#31363=CARTESIAN_POINT('Ctrl Pts',(-57.3551116946747,3.69650985244822,3.55406486819218));
#31364=CARTESIAN_POINT('Ctrl Pts',(-57.2158530505917,1.54011704282762,4.89117588296368));
#31365=CARTESIAN_POINT('Ctrl Pts',(-57.076594406509,-0.993339894845993,
5.03078900139859));
#31366=CARTESIAN_POINT('Ctrl Pts',(-56.937335762426,-3.28359918545446,3.93872294825806));
#31367=CARTESIAN_POINT('Ctrl Pts',(-56.8096011482596,-4.64694192022078,
2.05251707513984));
#31368=CARTESIAN_POINT('Ctrl Pts',(-56.7282860821206,-4.91757746258099,
0.616075270651702));
#31369=CARTESIAN_POINT('Ctrl Pts',(-56.6933905640093,-4.9182044571118,-0.000129187542790513));
#31370=CARTESIAN_POINT('Ctrl Pts',(-58.0981094359908,-4.91834149996792,
-0.000124244451390268));
#31371=CARTESIAN_POINT('Ctrl Pts',(-58.0890244848416,-4.91850756103116,
-0.160538493998118));
#31372=CARTESIAN_POINT('Ctrl Pts',(-58.0335199856648,-4.87150837253063,
-1.14049229247011));
#31373=CARTESIAN_POINT('Ctrl Pts',(-57.9315959384605,-4.23847415605518,
-2.88632966415425));
#31374=CARTESIAN_POINT('Ctrl Pts',(-57.7923372943776,-2.33586251016583,
-4.56500912177253));
#31375=CARTESIAN_POINT('Ctrl Pts',(-57.6530786502948,0.13863421179886,-5.12604551322175));
#31376=CARTESIAN_POINT('Ctrl Pts',(-57.5138200062119,2.57918936704391,-4.43208125010674));
#31377=CARTESIAN_POINT('Ctrl Pts',(-57.3745613621292,4.38828615879628,-2.65301839525271));
#31378=CARTESIAN_POINT('Ctrl Pts',(-57.2353027180462,5.12300662642812,-0.224421743812369));
#31379=CARTESIAN_POINT('Ctrl Pts',(-57.0960440739635,4.60347045903611,2.25911968355451));
#31380=CARTESIAN_POINT('Ctrl Pts',(-56.9567854298806,2.95687477625445,4.18956484277621));
#31381=CARTESIAN_POINT('Ctrl Pts',(-56.8175267857977,0.586352681285569,
5.09428626459846));
#31382=CARTESIAN_POINT('Ctrl Pts',(-56.678268141715,-1.92772510164183,4.75178260718661));
#31383=CARTESIAN_POINT('Ctrl Pts',(-56.539009497632,-3.96984136372351,3.24590843369777));
#31384=CARTESIAN_POINT('Ctrl Pts',(-56.428956595724,-4.81558555136314,1.42782549805425));
#31385=CARTESIAN_POINT('Ctrl Pts',(-56.3653232418436,-4.91813495580623,
0.304108969632793));
#31386=CARTESIAN_POINT('Ctrl Pts',(-56.3481094359908,-4.91793587170447,
9.03881743493859E-5));
#31387=CARTESIAN_POINT('Ctrl Pts',(-60.1597342437858,-2.14786219406457,
4.42446279878225));
#31388=CARTESIAN_POINT('Ctrl Pts',(-60.1133146957582,-2.8852624348776,4.06649073049583));
#31389=CARTESIAN_POINT('Ctrl Pts',(-60.0204755997031,-4.17685949869944,
2.97507394228249));
#31390=CARTESIAN_POINT('Ctrl Pts',(-59.8812169556201,-5.09175167965884,
0.607962263996158));
#31391=CARTESIAN_POINT('Ctrl Pts',(-59.7419583115374,-4.75996762098409,
-1.90732467562513));
#31392=CARTESIAN_POINT('Ctrl Pts',(-59.6026996674545,-3.26284724500757,
-3.95597454038308));
#31393=CARTESIAN_POINT('Ctrl Pts',(-59.4634410233716,-0.966870086247853,
-5.03592242336179));
#31394=CARTESIAN_POINT('Ctrl Pts',(-59.3241823792888,1.56581406446455,-4.88302020893749));
#31395=CARTESIAN_POINT('Ctrl Pts',(-59.184923735206,3.71514791027481,-3.53457280157081));
#31396=CARTESIAN_POINT('Ctrl Pts',(-59.0456650911232,4.95490602150955,-1.32078475768876));
#31397=CARTESIAN_POINT('Ctrl Pts',(-58.9064064470403,4.98156463212109,1.21638024324112));
#31398=CARTESIAN_POINT('Ctrl Pts',(-58.7671478029575,3.78859490309226,3.45573509562084));
#31399=CARTESIAN_POINT('Ctrl Pts',(-58.6278891588746,1.66807055469799,4.84903148731836));
#31400=CARTESIAN_POINT('Ctrl Pts',(-58.4886305147918,-0.860844735280108,
5.05514653385482));
#31401=CARTESIAN_POINT('Ctrl Pts',(-58.349371870709,-3.17900084006467,4.02361981064615));
#31402=CARTESIAN_POINT('Ctrl Pts',(-58.2101132266261,-4.71884785030005,
2.00699696920383));
#31403=CARTESIAN_POINT('Ctrl Pts',(-58.0708545825433,-5.10338767805891,
-0.500995174027796));
#31404=CARTESIAN_POINT('Ctrl Pts',(-57.9315959384605,-4.23847415605518,
-2.88632966415425));
#31405=CARTESIAN_POINT('Ctrl Pts',(-57.7923372943776,-2.33586251016583,
-4.56500912177253));
#31406=CARTESIAN_POINT('Ctrl Pts',(-57.6530786502948,0.13863421179886,-5.12604551322175));
#31407=CARTESIAN_POINT('Ctrl Pts',(-57.5138200062119,2.57918936704391,-4.43208125010674));
#31408=CARTESIAN_POINT('Ctrl Pts',(-57.3745613621292,4.38828615879628,-2.65301839525271));
#31409=CARTESIAN_POINT('Ctrl Pts',(-57.2353027180462,5.12300662642812,-0.224421743812369));
#31410=CARTESIAN_POINT('Ctrl Pts',(-57.0960440739635,4.60347045903611,2.25911968355451));
#31411=CARTESIAN_POINT('Ctrl Pts',(-56.9567854298806,2.95687477625445,4.18956484277621));
#31412=CARTESIAN_POINT('Ctrl Pts',(-56.8175267857977,0.586352681285569,
5.09428626459846));
#31413=CARTESIAN_POINT('Ctrl Pts',(-56.678268141715,-1.92772510164183,4.75178260718661));
#31414=CARTESIAN_POINT('Ctrl Pts',(-56.539009497632,-3.96984136372351,3.24590843369777));
#31415=CARTESIAN_POINT('Ctrl Pts',(-56.3997508535493,-5.04002839895529,
0.945344249943794));
#31416=CARTESIAN_POINT('Ctrl Pts',(-56.2604922094663,-4.87627421179875,
-1.58666689148564));
#31417=CARTESIAN_POINT('Ctrl Pts',(-56.1212335653836,-3.51867044972994,
-3.73021718930019));
#31418=CARTESIAN_POINT('Ctrl Pts',(-55.9819749213007,-1.29959683625502,
-4.96050502231166));
#31419=CARTESIAN_POINT('Ctrl Pts',(-55.8427162772179,1.23765476786001,-4.97632120032051));
#31420=CARTESIAN_POINT('Ctrl Pts',(-55.7034576331351,3.471893548184,-3.77379347649709));
#31421=CARTESIAN_POINT('Ctrl Pts',(-55.5641989890522,4.85611478302155,-1.64733458267922));
#31422=CARTESIAN_POINT('Ctrl Pts',(-55.4249403449694,5.0514220401755,0.882438318071356));
#31423=CARTESIAN_POINT('Ctrl Pts',(-55.2856817008865,4.00999858994569,3.19616540901837));
#31424=CARTESIAN_POINT('Ctrl Pts',(-55.1464230568037,1.98681429033347,4.72738098622251));
#31425=CARTESIAN_POINT('Ctrl Pts',(-55.0071644127208,-0.522798231506428,
5.10120025310764));
#31426=CARTESIAN_POINT('Ctrl Pts',(-54.867905768638,-2.90441498868291,4.22610170093973));
#31427=CARTESIAN_POINT('Ctrl Pts',(-54.7286471245552,-4.57494897056921,
2.31633415764206));
#31428=CARTESIAN_POINT('Ctrl Pts',(-54.5893884804724,-5.12540630243158,
-0.160537373113851));
#31429=CARTESIAN_POINT('Ctrl Pts',(-54.4501298363895,-4.42101949107612,
-2.59810482326958));
#31430=CARTESIAN_POINT('Ctrl Pts',(-54.3108711923067,-2.6342423114104,-4.39958287317637));
#31431=CARTESIAN_POINT('Ctrl Pts',(-54.1716125482239,-0.202528254306939,
-5.12391884394933));
#31432=CARTESIAN_POINT('Ctrl Pts',(-54.0323539041409,2.27877043643476,-4.59377484332902));
#31433=CARTESIAN_POINT('Ctrl Pts',(-53.8930952600582,4.20216179902152,-2.93894508761492));
#31434=CARTESIAN_POINT('Ctrl Pts',(-53.7538366159752,5.09674533424557,-0.564578613673673));
#31435=CARTESIAN_POINT('Ctrl Pts',(-53.6145779718925,4.74350174030785,1.94801264186554));
#31436=CARTESIAN_POINT('Ctrl Pts',(-53.4753193278096,3.22891502039301,3.98367541401808));
#31437=CARTESIAN_POINT('Ctrl Pts',(-53.3360606837268,0.923798757412272,
5.04402199330804));
#31438=CARTESIAN_POINT('Ctrl Pts',(-53.196802039644,-1.60748951844882,4.86944960557646));
#31439=CARTESIAN_POINT('Ctrl Pts',(-53.0575433955611,-3.74521898384984,
3.50269849918351));
#31440=CARTESIAN_POINT('Ctrl Pts',(-52.9182847514784,-4.96601312166083,
1.27838792573463));
#31441=CARTESIAN_POINT('Ctrl Pts',(-52.7790261073954,-4.97098706627025,
-1.25890809837161));
#31442=CARTESIAN_POINT('Ctrl Pts',(-52.6397674633126,-3.75892305563278,
-3.48798788343709));
#31443=CARTESIAN_POINT('Ctrl Pts',(-52.5005088192298,-1.62656857379318,
-4.86310977543383));
#31444=CARTESIAN_POINT('Ctrl Pts',(-52.3612501751469,0.904015809819905,
-5.04760511814933));
#31445=CARTESIAN_POINT('Ctrl Pts',(-52.2219915310641,3.21327160455789,-3.99630424373741));
#31446=CARTESIAN_POINT('Ctrl Pts',(-52.0827328869813,4.73582780601003,-1.96659528245999));
#31447=CARTESIAN_POINT('Ctrl Pts',(-51.9434742428983,5.09891967722156,0.544591717173908));
#31448=CARTESIAN_POINT('Ctrl Pts',(-51.8042155988156,4.21365207873328,2.92244729166469));
#31449=CARTESIAN_POINT('Ctrl Pts',(-51.6649569547327,2.29676350806032,4.58480527407807));
#31450=CARTESIAN_POINT('Ctrl Pts',(-51.5256983106499,-0.182437602611408,
5.12467350514402));
#31451=CARTESIAN_POINT('Ctrl Pts',(-51.3864396665671,-2.6169728383005,4.40987700245359));
#31452=CARTESIAN_POINT('Ctrl Pts',(-51.2471810224842,-4.41079925105322,
2.61541812719877));
#31453=CARTESIAN_POINT('Ctrl Pts',(-51.1079223784014,-5.12473749875106,
0.180631066171815));
#31454=CARTESIAN_POINT('Ctrl Pts',(-50.9686637343185,-4.58399534525111,
-2.29837957872232));
#31455=CARTESIAN_POINT('Ctrl Pts',(-50.8294050902357,-2.92096173384329,
-4.21468202390108));
#31456=CARTESIAN_POINT('Ctrl Pts',(-50.6901464461529,-0.542794236847172,
-5.09911133724467));
#31457=CARTESIAN_POINT('Ctrl Pts',(-50.55088780207,1.96826461136862,-4.73513425710461));
#31458=CARTESIAN_POINT('Ctrl Pts',(-50.4116291579872,3.99743672238916,-3.21186264707355));
#31459=CARTESIAN_POINT('Ctrl Pts',(-50.2723705139044,5.04792348380256,-0.902236396320984));
#31460=CARTESIAN_POINT('Ctrl Pts',(-50.1331118698215,4.86253608318979,1.62828279265274));
#31461=CARTESIAN_POINT('Ctrl Pts',(-49.9938532257387,3.48666258935134,3.76015239068703));
#31462=CARTESIAN_POINT('Ctrl Pts',(-49.8545945816558,1.25715567184686,4.97143054159615));
#31463=CARTESIAN_POINT('Ctrl Pts',(-49.7153359375731,-1.28013844121747,
4.96556216198015));
#31464=CARTESIAN_POINT('Ctrl Pts',(-49.5760772934901,-3.50401852802057,
3.74398399682213));
#31465=CARTESIAN_POINT('Ctrl Pts',(-49.4368186494073,-4.87001596744655,
1.60577286375978));
#31466=CARTESIAN_POINT('Ctrl Pts',(-49.2975600053245,-5.04369602683803,
-0.925576794236894));
#31467=CARTESIAN_POINT('Ctrl Pts',(-49.1583013612416,-3.98253692500126,
-3.23031912574798));
#31468=CARTESIAN_POINT('Ctrl Pts',(-49.0190427171589,-1.94634036455058,
-4.74418814956709));
#31469=CARTESIAN_POINT('Ctrl Pts',(-48.879784073076,0.566375258594887,-5.09654599504637));
#31470=CARTESIAN_POINT('Ctrl Pts',(-48.7405254289932,2.94042623074984,-4.20112551522683));
#31471=CARTESIAN_POINT('Ctrl Pts',(-48.6012667849103,4.5945778590284,-2.27715091956982));
#31472=CARTESIAN_POINT('Ctrl Pts',(-48.4620081408275,5.12384713130236,0.20433450079776));
#31473=CARTESIAN_POINT('Ctrl Pts',(-48.3227494967446,4.39865398946333,2.63579306739927));
#31474=CARTESIAN_POINT('Ctrl Pts',(-48.1834908526618,2.59654618544401,4.42193508772209));
#31475=CARTESIAN_POINT('Ctrl Pts',(-48.0442322085789,0.158730579712837,
5.12546257583017));
#31476=CARTESIAN_POINT('Ctrl Pts',(-47.9049735644962,-2.31794675259165,
4.57413214340397));
#31477=CARTESIAN_POINT('Ctrl Pts',(-47.7657149204133,-4.22712528867379,
2.90292504330135));
#31478=CARTESIAN_POINT('Ctrl Pts',(-47.6264562763305,-5.10138423045494,
0.520999948596248));
#31479=CARTESIAN_POINT('Ctrl Pts',(-47.4871976322476,-4.72668031033514,
-1.98848064035377));
#31480=CARTESIAN_POINT('Ctrl Pts',(-47.3479389881648,-3.1947516251322,-4.01112503755328));
#31481=CARTESIAN_POINT('Ctrl Pts',(-47.2086803440819,-0.880657560390307,
-5.05173279919862));
#31482=CARTESIAN_POINT('Ctrl Pts',(-47.0694216999991,1.6490463344078,-4.85553377087915));
#31483=CARTESIAN_POINT('Ctrl Pts',(-46.9301630559163,3.7750171371299,-3.47056301304949));
#31484=CARTESIAN_POINT('Ctrl Pts',(-46.7909044118334,4.97675718319434,-1.23590046229263));
#31485=CARTESIAN_POINT('Ctrl Pts',(-46.6516457677506,4.96004658650958,1.30134540873142));
#31486=CARTESIAN_POINT('Ctrl Pts',(-46.5123871236678,3.72897657285209,3.51998518921485));
#31487=CARTESIAN_POINT('Ctrl Pts',(-46.3731284795849,1.58494783230892,4.87683323295259));
#31488=CARTESIAN_POINT('Ctrl Pts',(-46.2338698355021,-0.947120877618752,
5.03969483762166));
#31489=CARTESIAN_POINT('Ctrl Pts',(-46.0946111914193,-3.24730766130082,
3.9686968851285));
#31490=CARTESIAN_POINT('Ctrl Pts',(-45.9553525473364,-4.75246186423383,
1.92604990646005));
#31491=CARTESIAN_POINT('Ctrl Pts',(-45.8160939032536,-5.09407924992551,
-0.588148458001959));
#31492=CARTESIAN_POINT('Ctrl Pts',(-45.6768352591708,-4.1885222391554,-2.95835147764295));
#31493=CARTESIAN_POINT('Ctrl Pts',(-45.5375766150878,-2.25749675029642,
-4.60426654697279));
#31494=CARTESIAN_POINT('Ctrl Pts',(-45.3983179710051,0.226227667835505,
-5.12292719599619));
#31495=CARTESIAN_POINT('Ctrl Pts',(-45.2590593269221,2.65456516690845,-4.38735065703757));
#31496=CARTESIAN_POINT('Ctrl Pts',(-45.1198006828394,4.43299017984253,-2.57762683074788));
#31497=CARTESIAN_POINT('Ctrl Pts',(-44.9805420387565,5.12609406194675,-0.136827194832999));
#31498=CARTESIAN_POINT('Ctrl Pts',(-44.8412833946737,4.56418541788972,2.33747160074608));
#31499=CARTESIAN_POINT('Ctrl Pts',(-44.7020247505909,2.88483534533912,4.23949136612563));
#31500=CARTESIAN_POINT('Ctrl Pts',(-44.562766106508,0.499196146884659,5.10356397237334));
#31501=CARTESIAN_POINT('Ctrl Pts',(-44.4235074624252,-2.00866035967626,
4.71814005436855));
#31502=CARTESIAN_POINT('Ctrl Pts',(-44.2842488183423,-4.02474010956177,
3.17758226701629));
#31503=CARTESIAN_POINT('Ctrl Pts',(-44.1449901742595,-5.05544986993808,
0.859062643649847));
#31504=CARTESIAN_POINT('Ctrl Pts',(-44.0057315301767,-4.8484427965068,-1.66977976457168));
#31505=CARTESIAN_POINT('Ctrl Pts',(-43.8664728860938,-3.45440006425625,
-3.78981295174814));
#31506=CARTESIAN_POINT('Ctrl Pts',(-43.7272142420111,-1.21462268519213,
-4.98199294919094));
#31507=CARTESIAN_POINT('Ctrl Pts',(-43.5879555979281,1.32252861367418,-4.95444044057296));
#31508=CARTESIAN_POINT('Ctrl Pts',(-43.4486969538454,3.53588757546868,-3.71390105775826));
#31509=CARTESIAN_POINT('Ctrl Pts',(-43.3094383097624,4.88356144746871,-1.56409385970568));
#31510=CARTESIAN_POINT('Ctrl Pts',(-43.1701796656797,5.03560162356189,0.968647666570477));
#31511=CARTESIAN_POINT('Ctrl Pts',(-43.0309210215968,3.95478437683829,3.26423690100571));
#31512=CARTESIAN_POINT('Ctrl Pts',(-42.891662377514,1.90572427869227,4.76064879893219));
#31513=CARTESIAN_POINT('Ctrl Pts',(-42.7524037334311,-0.60991091781632,
5.09151948690174));
#31514=CARTESIAN_POINT('Ctrl Pts',(-42.6131450893483,-2.97622270502889,
4.17584248065492));
#31515=CARTESIAN_POINT('Ctrl Pts',(-42.4738864452655,-4.61387116099574,
2.23780135912538));
#31516=CARTESIAN_POINT('Ctrl Pts',(-42.3346278011826,-5.12191371602353,
-0.248116703955333));
#31517=CARTESIAN_POINT('Ctrl Pts',(-42.1953691570999,-4.37596721157521,
-2.67328879404945));
#31518=CARTESIAN_POINT('Ctrl Pts',(-42.0561105130169,-2.5586604085778,-4.44396432554854));
#31519=CARTESIAN_POINT('Ctrl Pts',(-41.9168518689342,-0.114921311488126,
-5.12663194556987));
#31520=CARTESIAN_POINT('Ctrl Pts',(-41.7775932248512,2.35695376666187,-4.55415535033556));
#31521=CARTESIAN_POINT('Ctrl Pts',(-41.6383345807685,4.25178003045199,-2.86669297027451));
#31522=CARTESIAN_POINT('Ctrl Pts',(-41.4990759366856,5.10565052319778,-0.477383229849849));
#31523=CARTESIAN_POINT('Ctrl Pts',(-41.3598172926028,4.70951364514992,2.02880340085441));
#31524=CARTESIAN_POINT('Ctrl Pts',(-41.2205586485199,3.16035488623825,4.03828168980343));
#31525=CARTESIAN_POINT('Ctrl Pts',(-41.0813000044371,0.837452040422802,
5.05907462814725));
#31526=CARTESIAN_POINT('Ctrl Pts',(-40.9420413603542,-1.6904827045519,4.84126328955393));
#31527=CARTESIAN_POINT('Ctrl Pts',(-40.8027827162714,-3.80453956437015,
3.43817403810713));
#31528=CARTESIAN_POINT('Ctrl Pts',(-40.6635240721885,-4.98713774398085,
1.1933227290776));
#31529=CARTESIAN_POINT('Ctrl Pts',(-40.5242654281058,-4.9487438265385,-1.34368766924037));
#31530=CARTESIAN_POINT('Ctrl Pts',(-40.3850067840229,-3.69875772681961,
-3.5517253964044));
#31531=CARTESIAN_POINT('Ctrl Pts',(-40.2457481399401,-1.54321132674375,
-4.89020048813763));
#31532=CARTESIAN_POINT('Ctrl Pts',(-40.1064894958572,0.990156768012798,
-5.03141645940088));
#31533=CARTESIAN_POINT('Ctrl Pts',(-39.9672308517744,3.28110653573467,-3.9407996541731));
#31534=CARTESIAN_POINT('Ctrl Pts',(-39.8279722076915,4.76874880416872,-1.88536385239323));
#31535=CARTESIAN_POINT('Ctrl Pts',(-39.6887135636088,5.08886675271635,0.631662240655434));
#31536=CARTESIAN_POINT('Ctrl Pts',(-39.5494549195259,4.16308647125779,2.99403958657897));
#31537=CARTESIAN_POINT('Ctrl Pts',(-39.410196275443,2.21806510569457,4.62339152571701));
#31538=CARTESIAN_POINT('Ctrl Pts',(-39.2709376313602,-0.270001209463393,
5.12080670989053));
#31539=CARTESIAN_POINT('Ctrl Pts',(-39.1316789872773,-2.69196360692879,
4.36450386093798));
#31540=CARTESIAN_POINT('Ctrl Pts',(-38.9924203431946,-4.45485732445219,
2.53964726526075));
#31541=CARTESIAN_POINT('Ctrl Pts',(-38.8531616991117,-5.12707621687776,
0.0930133296797844));
#31542=CARTESIAN_POINT('Ctrl Pts',(-38.7139030550288,-4.5440421238906,-2.37639289459456));
#31543=CARTESIAN_POINT('Ctrl Pts',(-38.574644410946,-2.84849824938738,-4.26399105726181));
#31544=CARTESIAN_POINT('Ctrl Pts',(-38.4353857668631,-0.455561595795777,
-5.10764384482783));
#31545=CARTESIAN_POINT('Ctrl Pts',(-38.2961271227804,2.04890939607611,-4.70080124019754));
#31546=CARTESIAN_POINT('Ctrl Pts',(-38.1568684786975,4.05174953100885,-3.14306979737026));
#31547=CARTESIAN_POINT('Ctrl Pts',(-38.0176098346146,5.06260700763802,-0.815826145318977));
#31548=CARTESIAN_POINT('Ctrl Pts',(-37.8783511905319,4.83399538111841,1.71115477631265));
#31549=CARTESIAN_POINT('Ctrl Pts',(-37.7390925464489,3.42188523088942,3.81919670608788));
#31550=CARTESIAN_POINT('Ctrl Pts',(-37.5998339023662,1.17200098288635,4.99219147362009));
#31551=CARTESIAN_POINT('Ctrl Pts',(-37.4605752582833,-1.36482218906556,
4.94295684842645));
#31552=CARTESIAN_POINT('Ctrl Pts',(-37.3213166142005,-3.56749836282337,
3.68354685655336));
#31553=CARTESIAN_POINT('Ctrl Pts',(-37.1820579701177,-4.89675023373046,
1.52230061473821));
#31554=CARTESIAN_POINT('Ctrl Pts',(-37.0427993260348,-5.02713942155972,
-1.01164778918944));
#31555=CARTESIAN_POINT('Ctrl Pts',(-36.903540681952,-3.92674297249402,-3.29791625744811));
#31556=CARTESIAN_POINT('Ctrl Pts',(-36.7642820378691,-1.86496899934438,
-4.7767617320373));
#31557=CARTESIAN_POINT('Ctrl Pts',(-36.6250233937863,0.653402029340091,
-5.08612109580827));
#31558=CARTESIAN_POINT('Ctrl Pts',(-36.4857647497035,3.01180179695694,-4.15025444388879));
#31559=CARTESIAN_POINT('Ctrl Pts',(-36.3465061056206,4.63282746729464,-2.19828835038808));
#31560=CARTESIAN_POINT('Ctrl Pts',(-36.2072474615378,5.11960619781114,0.291880784748528));
#31561=CARTESIAN_POINT('Ctrl Pts',(-36.0679888174549,4.35296081444672,2.71058926454433));
#31562=CARTESIAN_POINT('Ctrl Pts',(-35.9287301733721,2.52058774797673,4.46566897764727));
#31563=CARTESIAN_POINT('Ctrl Pts',(-35.7894715292892,0.0711036494477585,
5.12742686775803));
#31564=CARTESIAN_POINT('Ctrl Pts',(-35.6502128852065,-2.39578862958558,
4.53384592322236));
#31565=CARTESIAN_POINT('Ctrl Pts',(-35.5109542411235,-4.27612422358166,
2.83025151491343));
#31566=CARTESIAN_POINT('Ctrl Pts',(-35.3716955970408,-5.10954390086544,
0.433731643185599));
#31567=CARTESIAN_POINT('Ctrl Pts',(-35.2324369529579,-4.69200299859993,
-2.0689779782059));
#31568=CARTESIAN_POINT('Ctrl Pts',(-35.0931783088751,-3.125727316038,-4.06514338725531));
#31569=CARTESIAN_POINT('Ctrl Pts',(-34.9539196647922,-0.794185353227152,
-5.06604694390913));
#31570=CARTESIAN_POINT('Ctrl Pts',(-34.8146610207094,1.73179560238191,-4.82663920391221));
#31571=CARTESIAN_POINT('Ctrl Pts',(-34.6754023766266,3.83378410926193,-3.40553394003679));
#31572=CARTESIAN_POINT('Ctrl Pts',(-34.5361437325437,4.99715404582752,-1.15065783595354));
#31573=CARTESIAN_POINT('Ctrl Pts',(-34.3968850884609,4.93707961190701,1.38593178723334));
#31574=CARTESIAN_POINT('Ctrl Pts',(-34.257626444378,3.6682687247101,3.58320618671119));
#31575=CARTESIAN_POINT('Ctrl Pts',(-34.1183678002952,1.5013621055187,4.90321056464884));
#31576=CARTESIAN_POINT('Ctrl Pts',(-33.9791091562124,-1.03312033767432,
5.02277058813713));
#31577=CARTESIAN_POINT('Ctrl Pts',(-33.8398505121295,-3.31466575920044,
3.91261458847608));
#31578=CARTESIAN_POINT('Ctrl Pts',(-33.7005918680467,-4.78468743622185,
1.84454009195584));
#31579=CARTESIAN_POINT('Ctrl Pts',(-33.5613332239638,-5.0832825663132,-0.675129886901675));
#31580=CARTESIAN_POINT('Ctrl Pts',(-33.422074579881,-4.13734663286075,-3.02950901182476));
#31581=CARTESIAN_POINT('Ctrl Pts',(-33.2828159357982,-2.17847145432949,
-4.64217881342837));
#31582=CARTESIAN_POINT('Ctrl Pts',(-33.1435572917154,0.313755030289582,
-5.11831220170669));
#31583=CARTESIAN_POINT('Ctrl Pts',(-33.0042986476325,2.72916542679145,-4.34133828287751));
#31584=CARTESIAN_POINT('Ctrl Pts',(-32.8650400035497,4.47639908771296,-2.50148220475266));
#31585=CARTESIAN_POINT('Ctrl Pts',(-32.7257813594668,5.12768389180779,-0.0491926708628662));
#31586=CARTESIAN_POINT('Ctrl Pts',(-32.586522715384,4.52356693451351,2.41514061746884));
#31587=CARTESIAN_POINT('Ctrl Pts',(-32.4472640713011,2.81195310003798,4.28817930785997));
#31588=CARTESIAN_POINT('Ctrl Pts',(-32.3080054272183,0.411893770634228,
5.11135065661556));
#31589=CARTESIAN_POINT('Ctrl Pts',(-32.1687467831355,-2.08900878079138,
4.68311908101302));
#31590=CARTESIAN_POINT('Ctrl Pts',(-32.0294881390527,-4.07846301397088,
3.10832775891526));
#31591=CARTESIAN_POINT('Ctrl Pts',(-31.8902294949698,-5.06939437414735,
0.772530059308323));
#31592=CARTESIAN_POINT('Ctrl Pts',(-31.750970850887,-4.81919489225918,-1.75240480585811));
#31593=CARTESIAN_POINT('Ctrl Pts',(-31.6117122068041,-3.38912046412381,
-3.84830150752625));
#31594=CARTESIAN_POINT('Ctrl Pts',(-31.4724535627214,-1.12929367800508,
-5.00202536998659));
#31595=CARTESIAN_POINT('Ctrl Pts',(-31.3331949186384,1.40701607828237,-4.93111222429854));
#31596=CARTESIAN_POINT('Ctrl Pts',(-31.1939362745556,3.59884858124293,-3.65292361026856));
#31597=CARTESIAN_POINT('Ctrl Pts',(-31.0546776304728,4.90958136292712,-1.48039618142248));
#31598=CARTESIAN_POINT('Ctrl Pts',(-30.9154189863899,5.01831003890801,1.05457402137864));
#31599=CARTESIAN_POINT('Ctrl Pts',(-30.7761603423071,3.89841476010363,3.33135473514573));
#31600=CARTESIAN_POINT('Ctrl Pts',(-30.6369016982242,1.82407750325954,4.79252577199894));
#31601=CARTESIAN_POINT('Ctrl Pts',(-30.4976430541415,-0.696845416589377,
5.08035121606272));
#31602=CARTESIAN_POINT('Ctrl Pts',(-30.3583844100586,-3.04716090784859,
4.12436327387041));
#31603=CARTESIAN_POINT('Ctrl Pts',(-30.2191257659758,-4.65144539336256,
2.15861477937539));
#31604=CARTESIAN_POINT('Ctrl Pts',(-30.0798671218929,-5.11692474520557,
-0.335623546662854));
#31605=CARTESIAN_POINT('Ctrl Pts',(-29.9406084778101,-4.32963647845777,
-2.74769175446946));
#31606=CARTESIAN_POINT('Ctrl Pts',(-29.8013498337272,-2.48233098445573,
-4.48704745871744));
#31607=CARTESIAN_POINT('Ctrl Pts',(-29.6620911896444,-0.0272807940196574,
-5.12784728433378));
#31608=CARTESIAN_POINT('Ctrl Pts',(-29.5228325455616,2.43444850487691,-4.5132053454584));
#31609=CARTESIAN_POINT('Ctrl Pts',(-29.3835739014787,4.30015608997081,-2.79360333889022));
#31610=CARTESIAN_POINT('Ctrl Pts',(-29.2443152573959,5.11306407908685,-0.390048376901321));
#31611=CARTESIAN_POINT('Ctrl Pts',(-29.105056613313,4.67414964965714,2.10900143807006));
#31612=CARTESIAN_POINT('Ctrl Pts',(-28.9657979692302,3.09087144371802,4.09170816793918));
#31613=CARTESIAN_POINT('Ctrl Pts',(-28.8265393251474,0.750860658988233,
5.07264923722855));
#31614=CARTESIAN_POINT('Ctrl Pts',(-28.6872806810645,-1.77298201041712,
4.81166258209249));
#31615=CARTESIAN_POINT('Ctrl Pts',(-28.5480220369817,-3.86274863579312,
3.37264510286066));
#31616=CARTESIAN_POINT('Ctrl Pts',(-28.4087633928988,-5.00680535714688,
1.10790889915052));
#31617=CARTESIAN_POINT('Ctrl Pts',(-28.269504748816,-4.92505479456558,-1.42807467721344));
#31618=CARTESIAN_POINT('Ctrl Pts',(-28.1302461047332,-3.63751179343058,
-3.61442526078837));
#31619=CARTESIAN_POINT('Ctrl Pts',(-27.9909874606504,-1.45940322528745,
-4.91586251223447));
#31620=CARTESIAN_POINT('Ctrl Pts',(-27.8517288165675,1.07600844855802,-5.01375785532204));
#31621=CARTESIAN_POINT('Ctrl Pts',(-27.7124701724847,3.34798288054322,-3.88414374666556));
#31622=CARTESIAN_POINT('Ctrl Pts',(-27.5732115284018,4.80027659624061,-1.80358160690233));
#31623=CARTESIAN_POINT('Ctrl Pts',(-27.433952884319,5.07732709858328,0.718548221877666));
#31624=CARTESIAN_POINT('Ctrl Pts',(-27.2946942402362,4.11130460399385,3.06475716270483));
#31625=CARTESIAN_POINT('Ctrl Pts',(-27.1554355961534,2.13871868810873,4.66062703788945));
#31626=CARTESIAN_POINT('Ctrl Pts',(-27.0161769520704,-0.357485934549103,
5.11544385364273));
#31627=CARTESIAN_POINT('Ctrl Pts',(-26.8769183079877,-2.76616790928751,
4.3178556148625));
#31628=CARTESIAN_POINT('Ctrl Pts',(-26.7376596639048,-4.49761389622142,
2.46313443678733));
#31629=CARTESIAN_POINT('Ctrl Pts',(-26.598401019822,-5.12791704235244,0.00536841902906056));
#31630=CARTESIAN_POINT('Ctrl Pts',(-26.4591423757392,-4.50276134525971,
-2.45371193924766));
#31631=CARTESIAN_POINT('Ctrl Pts',(-26.3198837316563,-2.77520256653693,
-4.31205435121805));
#31632=CARTESIAN_POINT('Ctrl Pts',(-26.1806250875735,-0.36819586088392,
-5.11468413699221));
#31633=CARTESIAN_POINT('Ctrl Pts',(-26.0413664434906,2.12895558497593,-4.6650948683142));
#31634=CARTESIAN_POINT('Ctrl Pts',(-25.9021077994078,4.10487860730363,-3.07335868919861));
#31635=CARTESIAN_POINT('Ctrl Pts',(-25.762849155325,5.07581147371895,-0.729177547950212));
#31636=CARTESIAN_POINT('Ctrl Pts',(-25.6235905112421,4.80404241095214,1.79352684031905));
#31637=CARTESIAN_POINT('Ctrl Pts',(-25.4843318671593,3.35610815708752,3.87712523025787));
#31638=CARTESIAN_POINT('Ctrl Pts',(-25.3450732230764,1.08650388987611,5.01149392002581));
#31639=CARTESIAN_POINT('Ctrl Pts',(-25.2058145789936,-1.44910719949644,
4.91890743331681));
#31640=CARTESIAN_POINT('Ctrl Pts',(-25.0665559349108,-3.62993594091732,
3.62203355561599));
#31641=CARTESIAN_POINT('Ctrl Pts',(-24.9272972908279,-4.9220538978771,1.43838362044503));
#31642=CARTESIAN_POINT('Ctrl Pts',(-24.7880386467451,-5.00911412050208,
-1.09742322781982));
#31643=CARTESIAN_POINT('Ctrl Pts',(-24.6487800026622,-3.86980180875062,
-3.36454989176295));
#31644=CARTESIAN_POINT('Ctrl Pts',(-24.5095213585794,-1.7830527771394,-4.80793976741671));
#31645=CARTESIAN_POINT('Ctrl Pts',(-24.3702627144966,0.740237906473115,
-5.07421026909526));
#31646=CARTESIAN_POINT('Ctrl Pts',(-24.2310040704137,3.08229745508568,-4.09817086168255));
#31647=CARTESIAN_POINT('Ctrl Pts',(-24.0917454263309,4.66972357935212,-2.11878354383227));
#31648=CARTESIAN_POINT('Ctrl Pts',(-23.9524867822481,5.11386955405928,0.379341794741001));
#31649=CARTESIAN_POINT('Ctrl Pts',(-23.8132281381652,4.30599590721036,2.78459355387089));
#31650=CARTESIAN_POINT('Ctrl Pts',(-23.6739694940824,2.44389291227653,4.50809820728166));
#31651=CARTESIAN_POINT('Ctrl Pts',(-23.5347108499995,-0.0165440539888569,
5.12789316459004));
#31652=CARTESIAN_POINT('Ctrl Pts',(-23.3954522059167,-2.47293056883089,
4.49223512462487));
#31653=CARTESIAN_POINT('Ctrl Pts',(-23.2561935618339,-4.32387387433953,
2.75675111897605));
#31654=CARTESIAN_POINT('Ctrl Pts',(-23.116934917751,-5.11621080074934,0.346336621608935));
#31655=CARTESIAN_POINT('Ctrl Pts',(-22.9776762736682,-4.65595490232451,
-2.14887085714615));
#31656=CARTESIAN_POINT('Ctrl Pts',(-22.8384176295854,-3.05578981514007,
-4.11797409157195));
#31657=CARTESIAN_POINT('Ctrl Pts',(-22.6991589855025,-0.707481122127949,
-5.0788810258761));
#31658=CARTESIAN_POINT('Ctrl Pts',(-22.5599003414197,1.81403892041534,-4.79633451798247));
#31659=CARTESIAN_POINT('Ctrl Pts',(-22.4206416973369,3.89143102840395,-3.33950992876898));
#31660=CARTESIAN_POINT('Ctrl Pts',(-22.281383053254,5.01609097301024,-1.06507904103722));
#31661=CARTESIAN_POINT('Ctrl Pts',(-22.1421244091712,4.91267025280302,1.47011326107748));
#31662=CARTESIAN_POINT('Ctrl Pts',(-22.0028657650884,3.60648917945748,3.64538033840472));
#31663=CARTESIAN_POINT('Ctrl Pts',(-21.8636071210055,1.41733775071325,4.92815540680027));
#31664=CARTESIAN_POINT('Ctrl Pts',(-21.7243484769227,-1.11881796813,5.00437891924276));
#31665=CARTESIAN_POINT('Ctrl Pts',(-21.5850898328398,-3.38105546629115,
3.85538920824271));
#31666=CARTESIAN_POINT('Ctrl Pts',(-21.445831188757,-4.81551514559774,1.7624913888273));
#31667=CARTESIAN_POINT('Ctrl Pts',(-21.3065725446742,-5.07100078451202,
-0.761914074322125));
#31668=CARTESIAN_POINT('Ctrl Pts',(-21.1673139005913,-4.08496228675852,
-3.0997814647056));
#31669=CARTESIAN_POINT('Ctrl Pts',(-21.0280552565085,-2.09880971056153,
-4.67873485164786));
#31670=CARTESIAN_POINT('Ctrl Pts',(-20.8887966124256,0.401190728150701,
-5.11220187520187));
#31671=CARTESIAN_POINT('Ctrl Pts',(-20.7495379683428,2.80296835176735,-4.29405757205957));
#31672=CARTESIAN_POINT('Ctrl Pts',(-20.61027932426,4.51850020045465,-2.4246067622736));
#31673=CARTESIAN_POINT('Ctrl Pts',(-20.4710206801771,5.12777565148253,0.0384562249122501));
#31674=CARTESIAN_POINT('Ctrl Pts',(-20.3317620360943,4.48162687576275,2.49210404269421));
#31675=CARTESIAN_POINT('Ctrl Pts',(-20.1925033920114,2.7382493331312,4.33561444351065));
#31676=CARTESIAN_POINT('Ctrl Pts',(-20.0532447479286,0.324471058226111,
5.11764404248138));
#31677=CARTESIAN_POINT('Ctrl Pts',(-19.9139861038458,-2.16874689092793,
4.64672991858383));
#31678=CARTESIAN_POINT('Ctrl Pts',(-19.774727459763,-4.13099438162065,3.03816514234996));
#31679=CARTESIAN_POINT('Ctrl Pts',(-19.6354688156801,-5.08185783764996,
0.6857717776981));
#31680=CARTESIAN_POINT('Ctrl Pts',(-19.4962101715973,-4.78853904392961,
-1.83451787615531));
#31681=CARTESIAN_POINT('Ctrl Pts',(-19.3569515275144,-3.32285072098886,
-3.90566576900731));
#31682=CARTESIAN_POINT('Ctrl Pts',(-19.2176928834316,-1.04363474385184,
-5.02059643215792));
#31683=CARTESIAN_POINT('Ctrl Pts',(-19.0784342393487,1.49109247838584,-4.90634336691521));
#31684=CARTESIAN_POINT('Ctrl Pts',(-18.9391755952659,3.66075817123595,-3.59087894879527));
#31685=CARTESIAN_POINT('Ctrl Pts',(-18.7999169511831,4.93416692759049,-1.39626600038956));
#31686=CARTESIAN_POINT('Ctrl Pts',(-18.6606583071003,4.99955233800879,1.14019227882075));
#31687=CARTESIAN_POINT('Ctrl Pts',(-18.5213996630174,3.84090620831584,3.39749930273613));
#31688=CARTESIAN_POINT('Ctrl Pts',(-18.3821410189346,1.74189781741689,4.82300259245731));
#31689=CARTESIAN_POINT('Ctrl Pts',(-18.2428823748517,-0.783576329617824,
5.0676987034387));
#31690=CARTESIAN_POINT('Ctrl Pts',(-18.1036237307689,-3.11720887230625,
4.0716791204105));
#31691=CARTESIAN_POINT('Ctrl Pts',(-17.9643650866861,-4.68766069023061,
2.07879755301915));
#31692=CARTESIAN_POINT('Ctrl Pts',(-17.8251064426032,-5.11044084752239,
-0.423032335816314));
#31693=CARTESIAN_POINT('Ctrl Pts',(-17.6858477985204,-4.28204082740422,
-2.82129196745304));
#31694=CARTESIAN_POINT('Ctrl Pts',(-17.5465891544375,-2.40527633894355,
-4.52881968580006));
#31695=CARTESIAN_POINT('Ctrl Pts',(-17.4073305103547,0.0603676936250531,
-5.12756450517573));
#31696=CARTESIAN_POINT('Ctrl Pts',(-17.2680718662719,2.51123201073006,-4.4709367923799));
#31697=CARTESIAN_POINT('Ctrl Pts',(-17.128813222189,4.34727584434856,-2.71969754684507));
#31698=CARTESIAN_POINT('Ctrl Pts',(-16.9895545781062,5.11898383601734,-0.302599570000859));
#31699=CARTESIAN_POINT('Ctrl Pts',(-16.8502959340234,4.63742008554047,2.18858332338469));
#31700=CARTESIAN_POINT('Ctrl Pts',(-16.7110372899405,3.02048499265497,4.14393923969909));
#31701=CARTESIAN_POINT('Ctrl Pts',(-16.5717786458577,0.664049911073469,
5.08474185468397));
#31702=CARTESIAN_POINT('Ctrl Pts',(-16.4325200017749,-1.85496333359322,
4.78065613113894));
#31703=CARTESIAN_POINT('Ctrl Pts',(-16.293261357692,-3.91982919214168,3.30613083794419));
#31704=CARTESIAN_POINT('Ctrl Pts',(-16.1540027136092,-5.02501021519924,
1.02217138989266));
#31705=CARTESIAN_POINT('Ctrl Pts',(-16.0147440695263,-4.89992689118224,
-1.51204446834105));
#31706=CARTESIAN_POINT('Ctrl Pts',(-15.8754854254435,-3.57520314867229,
-3.6760691586116));
#31707=CARTESIAN_POINT('Ctrl Pts',(-15.7362267813606,-1.37516875424451,
-4.94008835047726));
#31708=CARTESIAN_POINT('Ctrl Pts',(-15.5969681372778,1.16154576959681,-4.99463446493368));
#31709=CARTESIAN_POINT('Ctrl Pts',(-15.457709493195,3.41388110083322,-3.82635307342976));
#31710=CARTESIAN_POINT('Ctrl Pts',(-15.3184508491121,4.83040197127458,-1.72127243894698));
#31711=CARTESIAN_POINT('Ctrl Pts',(-15.1791922050293,5.06430408617135,0.805224276807312));
#31712=CARTESIAN_POINT('Ctrl Pts',(-15.0399335609465,4.05832160518909,3.13457935966327));
#31713=CARTESIAN_POINT('Ctrl Pts',(-14.9006749168636,2.05874743662691,4.69650093211465));
#31714=CARTESIAN_POINT('Ctrl Pts',(-14.7614162727808,-0.444866218910259,
5.10858650317719));
#31715=CARTESIAN_POINT('Ctrl Pts',(-14.622157628698,-2.83956406633868,4.26994589267004));
#31716=CARTESIAN_POINT('Ctrl Pts',(-14.4828989846151,-4.53905647488387,
2.38590199526017));
#31717=CARTESIAN_POINT('Ctrl Pts',(-14.3436403405323,-5.12725972952516,
-0.0822780600233842));
#31718=CARTESIAN_POINT('Ctrl Pts',(-14.2043816964495,-4.46016506967744,
-2.5303141236615));
#31719=CARTESIAN_POINT('Ctrl Pts',(-14.0651230523666,-2.70109609887331,
-4.35885786391608));
#31720=CARTESIAN_POINT('Ctrl Pts',(-13.9258644082838,-0.280722556306372,
-5.12023015689262));
#31721=CARTESIAN_POINT('Ctrl Pts',(-13.7866057642009,2.20837979230334,-4.62802557319187));
#31722=CARTESIAN_POINT('Ctrl Pts',(-13.6473471201181,4.15680842943421,-3.00274968889455));
#31723=CARTESIAN_POINT('Ctrl Pts',(-13.5080884760352,5.08753302431593,-0.642315918895402));
#31724=CARTESIAN_POINT('Ctrl Pts',(-13.3688298319524,4.7726859235525,1.87537491939491));
#31725=CARTESIAN_POINT('Ctrl Pts',(-13.2295711878696,3.28935058494016,3.93392103918285));
#31726=CARTESIAN_POINT('Ctrl Pts',(-13.0903125437867,1.00068937108082,5.02933224153838));
#31727=CARTESIAN_POINT('Ctrl Pts',(-12.9510538997039,-1.5329688483594,4.89342094276911));
#31728=CARTESIAN_POINT('Ctrl Pts',(-12.8117952556211,-3.69131302095292,
3.55946206532884));
#31729=CARTESIAN_POINT('Ctrl Pts',(-12.6725366115382,-4.94591956733545,
1.35404639751376));
#31730=CARTESIAN_POINT('Ctrl Pts',(-12.5332779674554,-4.98962538981774,
-1.18287805054368));
#31731=CARTESIAN_POINT('Ctrl Pts',(-12.3940193233725,-3.81173006932457,
-3.43020056145098));
#31732=CARTESIAN_POINT('Ctrl Pts',(-12.2547606792897,-1.70061563003689,
-4.83771314693687));
#31733=CARTESIAN_POINT('Ctrl Pts',(-12.1155020352069,0.826857520598954,
-5.06081699469566));
#31734=CARTESIAN_POINT('Ctrl Pts',(-11.9762433911241,3.1518926095914,-4.04488998500265));
#31735=CARTESIAN_POINT('Ctrl Pts',(-11.8369847470412,4.70525541587707,-2.03865972750019));
#31736=CARTESIAN_POINT('Ctrl Pts',(-11.6977261029584,5.10663887602661,0.466691978745618));
#31737=CARTESIAN_POINT('Ctrl Pts',(-11.5584674588755,4.25777298871062,2.85778431477567));
#31738=CARTESIAN_POINT('Ctrl Pts',(-11.4192088147927,2.36648408499891,4.54921038078241));
#31739=CARTESIAN_POINT('Ctrl Pts',(-11.2799501707098,-0.104186924024186,
5.12686133009603));
#31740=CARTESIAN_POINT('Ctrl Pts',(-11.140691526627,-2.54935003304931,4.44931190434692));
#31741=CARTESIAN_POINT('Ctrl Pts',(-11.0014328825442,-4.37036029072556,
2.68244532887828));
#31742=CARTESIAN_POINT('Ctrl Pts',(-10.8621742384613,-5.1213829823493,0.258840416617134));
#31743=CARTESIAN_POINT('Ctrl Pts',(-10.7229155943785,-4.61854655308201,
-2.22813593619999));
#31744=CARTESIAN_POINT('Ctrl Pts',(-10.5836569502957,-2.98495955491563,
-4.16960171583444));
#31745=CARTESIAN_POINT('Ctrl Pts',(-10.4443983062128,-0.620570198026758,
-5.09023129557908));
#31746=CARTESIAN_POINT('Ctrl Pts',(-10.30513966213,1.89575226084471,-4.76462856670633));
#31747=CARTESIAN_POINT('Ctrl Pts',(-10.1658810180471,3.94794105281364,-3.27251026838425));
#31748=CARTESIAN_POINT('Ctrl Pts',(-10.0266223739643,5.03356243225522,-0.979189079677917));
#31749=CARTESIAN_POINT('Ctrl Pts',(-9.88736372988145,4.88682564047436,1.55386523636191));
#31750=CARTESIAN_POINT('Ctrl Pts',(-9.74810508579864,3.54365598619697,3.7064894799071));
#31751=CARTESIAN_POINT('Ctrl Pts',(-9.6088464417158,1.33289931589153,4.95166047168699));
#31752=CARTESIAN_POINT('Ctrl Pts',(-9.46958779763295,-1.20418873213356,
4.98452520412669));
#31753=CARTESIAN_POINT('Ctrl Pts',(-9.33032915355013,-3.44645738659569,
3.79703746301662));
#31754=CARTESIAN_POINT('Ctrl Pts',(-9.19107050946728,-4.84493598594207,
1.67992776788027));
#31755=CARTESIAN_POINT('Ctrl Pts',(-9.05181186538445,-5.05723749268599,
-0.848475665969715));
#31756=CARTESIAN_POINT('Ctrl Pts',(-8.9125532213016,-4.03138450511247,-3.16914830595081));
#31757=CARTESIAN_POINT('Ctrl Pts',(-8.77329457721876,-2.01853479244033,
-4.71392398166109));
#31758=CARTESIAN_POINT('Ctrl Pts',(-8.63403593313593,0.488509216784092,
-5.10459800163426));
#31759=CARTESIAN_POINT('Ctrl Pts',(-8.49477728905309,2.87595238006221,-4.24552233780323));
#31760=CARTESIAN_POINT('Ctrl Pts',(-8.35551864497026,4.5592812180853,-2.34702296273093));
#31761=CARTESIAN_POINT('Ctrl Pts',(-8.21626000088742,5.1263693141631,0.126093885571429));
#31762=CARTESIAN_POINT('Ctrl Pts',(-8.07700135680457,4.43837749456725,2.56833939129752));
#31763=CARTESIAN_POINT('Ctrl Pts',(-7.93774271272176,2.66374557742339,4.38178291474247));
#31764=CARTESIAN_POINT('Ctrl Pts',(-7.7984840686389,0.236953550501235,5.12244229133686));
#31765=CARTESIAN_POINT('Ctrl Pts',(-7.65922542455607,-2.24785139432755,
4.60898319829779));
#31766=CARTESIAN_POINT('Ctrl Pts',(-7.51996678047323,-4.18231886529451,
2.96711491556586));
#31767=CARTESIAN_POINT('Ctrl Pts',(-7.38070813639039,-5.09283661920301,
0.598813145544185));
#31768=CARTESIAN_POINT('Ctrl Pts',(-7.24144949230755,-4.75648420772767,
-1.91609498585244));
#31769=CARTESIAN_POINT('Ctrl Pts',(-7.10219084822472,-3.25561019578073,
-3.96188897702852));
#31770=CARTESIAN_POINT('Ctrl Pts',(-6.96293220414188,-0.957670908279476,
-5.03770071010642));
#31771=CARTESIAN_POINT('Ctrl Pts',(-6.82367356005904,1.57473325078029,-4.88014110472828));
#31772=CARTESIAN_POINT('Ctrl Pts',(-6.68441491597621,3.72159825835185,-3.52778519989586));
#31773=CARTESIAN_POINT('Ctrl Pts',(-6.54515627189337,4.95731095870299,-1.31172789552367));
#31774=CARTESIAN_POINT('Ctrl Pts',(-6.40589762781053,4.97933400098995,1.22547742523351));
#31775=CARTESIAN_POINT('Ctrl Pts',(-6.26663898372769,3.78227552279275,3.46265127941791));
#31776=CARTESIAN_POINT('Ctrl Pts',(-6.12738033964487,1.65920923023726,4.8520703564012));
#31777=CARTESIAN_POINT('Ctrl Pts',(-5.988121695562,-0.870078318172324,5.05356564550398));
#31778=CARTESIAN_POINT('Ctrl Pts',(-5.84886305147918,-3.18634613365232,
4.01780541212868));
#31779=CARTESIAN_POINT('Ctrl Pts',(-5.70960440739635,-4.7225064711785,1.99837299892905));
#31780=CARTESIAN_POINT('Ctrl Pts',(-5.57034576331351,-5.10246391726663,
-0.510317534642611));
#31781=CARTESIAN_POINT('Ctrl Pts',(-5.43108711923067,-4.23319416364483,
-2.89406793044928));
#31782=CARTESIAN_POINT('Ctrl Pts',(-5.29182847514784,-2.32751898381641,
-4.56926880289899));
#31783=CARTESIAN_POINT('Ctrl Pts',(-5.15256983106498,0.147998544643936,
-5.12578369071063));
#31784=CARTESIAN_POINT('Ctrl Pts',(-5.01331118698215,2.58728185166053,-4.42736204000073));
#31785=CARTESIAN_POINT('Ctrl Pts',(-4.87405254289932,4.39312552738983,-2.64499718596595));
#31786=CARTESIAN_POINT('Ctrl Pts',(-4.73479389881648,5.12340806451229,-0.215062357612596));
#31787=CARTESIAN_POINT('Ctrl Pts',(-4.59553525473364,4.59933568346607,2.26752580668157));
#31788=CARTESIAN_POINT('Ctrl Pts',(-4.45627661065081,2.94921609668853,4.19495964559934));
#31789=CARTESIAN_POINT('Ctrl Pts',(-4.31701796656797,0.57704515873205,5.09534894761389));
#31790=CARTESIAN_POINT('Ctrl Pts',(-4.17775932248513,-1.93640272295992,
4.74825299533382));
#31791=CARTESIAN_POINT('Ctrl Pts',(-4.03850067840229,-3.97576455713786,
3.2386506757228));
#31792=CARTESIAN_POINT('Ctrl Pts',(-3.89924203431946,-5.04174699952815,
0.936135249811344));
#31793=CARTESIAN_POINT('Ctrl Pts',(-3.75998339023661,-4.87336745758836,
-1.59557251057302));
#31794=CARTESIAN_POINT('Ctrl Pts',(-3.62072474615378,-3.51184999623001,
-3.73663908038491));
#31795=CARTESIAN_POINT('Ctrl Pts',(-3.48146610207094,-1.29053252299245,
-4.96287092523671));
#31796=CARTESIAN_POINT('Ctrl Pts',(-3.3422074579881,1.24674374109644,-4.97405187513803));
#31797=CARTESIAN_POINT('Ctrl Pts',(-3.20294881390526,3.47878194424713,-3.76744451832491));
#31798=CARTESIAN_POINT('Ctrl Pts',(-3.06369016982243,4.8591161279818,-1.63846039519689));
#31799=CARTESIAN_POINT('Ctrl Pts',(-2.92443152573959,5.04980152031218,0.891665082289887));
#31800=CARTESIAN_POINT('Ctrl Pts',(-2.78517288165675,4.0041529537823,3.20348577954525));
#31801=CARTESIAN_POINT('Ctrl Pts',(-2.64591423757392,1.9781747155564,4.73100272599303));
#31802=CARTESIAN_POINT('Ctrl Pts',(-2.50665559349108,-0.532116534951586,
5.10023666524732));
#31803=CARTESIAN_POINT('Ctrl Pts',(-2.36739694940823,-2.91213063348896,
4.22078868480285));
#31804=CARTESIAN_POINT('Ctrl Pts',(-2.2281383053254,-4.57917295608466,2.30797251716464));
#31805=CARTESIAN_POINT('Ctrl Pts',(-2.08887966124257,-5.12510446412278,
-0.169900526165591));
#31806=CARTESIAN_POINT('Ctrl Pts',(-1.94962101715972,-4.41626575409672,
-2.60617701967216));
#31807=CARTESIAN_POINT('Ctrl Pts',(-1.8103623730769,-2.62620047284534,-4.40438801630634));
#31808=CARTESIAN_POINT('Ctrl Pts',(-1.67110372899405,-0.193167284512309,
-5.12428009940892));
#31809=CARTESIAN_POINT('Ctrl Pts',(-1.53184508491121,2.28715890535059,-4.58960454528829));
#31810=CARTESIAN_POINT('Ctrl Pts',(-1.39258644082838,4.20752364775137,-2.93126272184108));
#31811=CARTESIAN_POINT('Ctrl Pts',(-1.25332779674554,5.0977685824936,-0.555268006901366));
#31812=CARTESIAN_POINT('Ctrl Pts',(-1.1140691526627,4.73993440187225,1.95667777727522));
#31813=CARTESIAN_POINT('Ctrl Pts',(-0.974810508579856,3.22163334032844,
3.98956232001804));
#31814=CARTESIAN_POINT('Ctrl Pts',(-0.835551864497027,0.914579917925479,
5.04571140862161));
#31815=CARTESIAN_POINT('Ctrl Pts',(-0.696293220414185,-1.61637760332782,
4.86648495952254));
#31816=CARTESIAN_POINT('Ctrl Pts',(-0.55703457633135,-3.75162148741517,
3.49588943240163));
#31817=CARTESIAN_POINT('Ctrl Pts',(-0.417775932248522,-4.96832111478826,
1.26923775212314));
#31818=CARTESIAN_POINT('Ctrl Pts',(-0.278517288165672,-4.96871636595204,
-1.26783711748493));
#31819=CARTESIAN_POINT('Ctrl Pts',(-0.139258644082833,-3.75247085555401,
-3.49516562013044));
#31820=CARTESIAN_POINT('Ctrl Pts',(-0.0464195480276115,-2.32937887075175,
-4.40852359138744));
#31821=CARTESIAN_POINT('Ctrl Pts',(0.,-1.55153804394499,-4.66710967952236));
#31822=CARTESIAN_POINT('Ctrl Pts',(-59.9675728291906,-2.29321473482431,
4.72388001049939));
#31823=CARTESIAN_POINT('Ctrl Pts',(-59.921153281163,-3.08051715225516,4.3416828546863));
#31824=CARTESIAN_POINT('Ctrl Pts',(-59.8283141851078,-4.45952062202937,
3.1764064847768));
#31825=CARTESIAN_POINT('Ctrl Pts',(-59.6890555410249,-5.43632641336422,
0.649104968589505));
#31826=CARTESIAN_POINT('Ctrl Pts',(-59.549796896942,-5.08208949153779,-2.03639929150226));
#31827=CARTESIAN_POINT('Ctrl Pts',(-59.4105382528593,-3.48365430538738,
-4.22368768893344));
#31828=CARTESIAN_POINT('Ctrl Pts',(-59.2712796087763,-1.03230120376032,
-5.37671901698262));
#31829=CARTESIAN_POINT('Ctrl Pts',(-59.1320209646936,1.67177759101493,-5.21346943231462));
#31830=CARTESIAN_POINT('Ctrl Pts',(-58.9927623206106,3.96656356885327,-3.77376837874884));
#31831=CARTESIAN_POINT('Ctrl Pts',(-58.8535036765279,5.29021998226643,-1.41016638601528));
#31832=CARTESIAN_POINT('Ctrl Pts',(-58.714245032445,5.31868266429192,1.29869649210185));
#31833=CARTESIAN_POINT('Ctrl Pts',(-58.5749863883622,4.04498094899183,3.68959547908911));
#31834=CARTESIAN_POINT('Ctrl Pts',(-58.4357277442793,1.78095409720902,5.1771805877835));
#31835=CARTESIAN_POINT('Ctrl Pts',(-58.2964691001966,-0.919100786258854,
5.39724408305449));
#31836=CARTESIAN_POINT('Ctrl Pts',(-58.1572104561136,-3.39413375243565,
4.29591072583816));
#31837=CARTESIAN_POINT('Ctrl Pts',(-58.0179518120309,-5.03818701758687,
2.14281672038556));
#31838=CARTESIAN_POINT('Ctrl Pts',(-57.8786931679479,-5.44874985610609,
-0.534899081668944));
#31839=CARTESIAN_POINT('Ctrl Pts',(-57.7394345238652,-4.52530493562246,
-3.08165660426907));
#31840=CARTESIAN_POINT('Ctrl Pts',(-57.6001758797823,-2.49393761929334,
-4.87393754198233));
#31841=CARTESIAN_POINT('Ctrl Pts',(-57.4609172356995,0.148016021757186,
-5.47294101771703));
#31842=CARTESIAN_POINT('Ctrl Pts',(-57.3216585916167,2.75373116429528,-4.73201402621145));
#31843=CARTESIAN_POINT('Ctrl Pts',(-57.1823999475338,4.68525518433443,-2.83255643335289));
#31844=CARTESIAN_POINT('Ctrl Pts',(-57.043141303451,5.46969647996603,-0.239609063908964));
#31845=CARTESIAN_POINT('Ctrl Pts',(-56.9038826593682,4.91500167802301,2.41200136599783));
#31846=CARTESIAN_POINT('Ctrl Pts',(-56.7646240152853,3.15697572436193,4.47308577640863));
#31847=CARTESIAN_POINT('Ctrl Pts',(-56.6253653712025,0.626032997947133,
5.43903252158022));
#31848=CARTESIAN_POINT('Ctrl Pts',(-56.4861067271197,-2.05818027804203,
5.07335057230125));
#31849=CARTESIAN_POINT('Ctrl Pts',(-56.3468480830367,-4.23849292350452,
3.46556919182964));
#31850=CARTESIAN_POINT('Ctrl Pts',(-56.207589438954,-5.38110285676427,1.00931864690527));
#31851=CARTESIAN_POINT('Ctrl Pts',(-56.0683307948711,-5.20626691248704,
-1.69404159394754));
#31852=CARTESIAN_POINT('Ctrl Pts',(-55.9290721507884,-3.75678986510833,
-3.98265263303982));
#31853=CARTESIAN_POINT('Ctrl Pts',(-55.7898135067054,-1.38754461178488,
-5.2961978849341));
#31854=CARTESIAN_POINT('Ctrl Pts',(-55.6505548626227,1.32141073022532,-5.31308439309028));
#31855=CARTESIAN_POINT('Ctrl Pts',(-55.5112962185397,3.70684742458739,-4.02917786364572));
#31856=CARTESIAN_POINT('Ctrl Pts',(-55.372037574457,5.18474323222248,-1.75881485722158));
#31857=CARTESIAN_POINT('Ctrl Pts',(-55.232778930374,5.39326754125922,0.942155674217395));
#31858=CARTESIAN_POINT('Ctrl Pts',(-55.0935202862913,4.28136771460451,3.41245990136191));
#31859=CARTESIAN_POINT('Ctrl Pts',(-54.9542616422084,2.12126821662139,5.0472976174595));
#31860=CARTESIAN_POINT('Ctrl Pts',(-54.8150029981255,-0.558177620120985,
5.44641440127875));
#31861=CARTESIAN_POINT('Ctrl Pts',(-54.6757443540428,-3.10096581917486,
4.51209519783989));
#31862=CARTESIAN_POINT('Ctrl Pts',(-54.5364857099599,-4.88455005138143,
2.47308772218258));
#31863=CARTESIAN_POINT('Ctrl Pts',(-54.3972270658771,-5.47225854953695,
-0.171401438384739));
#31864=CARTESIAN_POINT('Ctrl Pts',(-54.2579684217942,-4.72020368341004,
-2.77392668850185));
#31865=CARTESIAN_POINT('Ctrl Pts',(-54.1187097777114,-2.812509713294,-4.69731638264738));
#31866=CARTESIAN_POINT('Ctrl Pts',(-53.9794511336286,-0.216233973612521,
-5.47067043009504));
#31867=CARTESIAN_POINT('Ctrl Pts',(-53.8401924895457,2.43298194667935,-4.90464992972923));
#31868=CARTESIAN_POINT('Ctrl Pts',(-53.7009338454629,4.48653520801346,-3.13783267771182));
#31869=CARTESIAN_POINT('Ctrl Pts',(-53.56167520138,5.4416580041481,-0.602785411196621));
#31870=CARTESIAN_POINT('Ctrl Pts',(-53.4224165572971,5.06450931330617,2.07984073945473));
#31871=CARTESIAN_POINT('Ctrl Pts',(-53.2831579132145,3.44742578118945,4.2532631671754));
#31872=CARTESIAN_POINT('Ctrl Pts',(-53.1438992691315,0.986315103624491,
5.38536671011573));
#31873=CARTESIAN_POINT('Ctrl Pts',(-53.0046406250487,-1.71627335309004,
5.19898046385382));
#31874=CARTESIAN_POINT('Ctrl Pts',(-52.8653819809658,-3.99866964586547,
3.73973704280055));
#31875=CARTESIAN_POINT('Ctrl Pts',(-52.726123336883,-5.30207873456371,1.3649004280708));
#31876=CARTESIAN_POINT('Ctrl Pts',(-52.5868646928002,-5.30738928153452,
-1.34410233997011));
#31877=CARTESIAN_POINT('Ctrl Pts',(-52.4476060487173,-4.01330111497288,
-3.72403091375702));
#31878=CARTESIAN_POINT('Ctrl Pts',(-52.3083474046345,-1.73664354767827,
-5.19221159761117));
#31879=CARTESIAN_POINT('Ctrl Pts',(-52.1690887605516,0.965193382202131,
-5.38919231620228));
#31880=CARTESIAN_POINT('Ctrl Pts',(-52.0298301164688,3.43072372656281,-4.26674662923164));
#31881=CARTESIAN_POINT('Ctrl Pts',(-51.890571472386,5.05631605991481,-2.09968092535702));
#31882=CARTESIAN_POINT('Ctrl Pts',(-51.7513128283031,5.44397949170202,0.581445939007525));
#31883=CARTESIAN_POINT('Ctrl Pts',(-51.6120541842203,4.49880307082833,3.12021842440015));
#31884=CARTESIAN_POINT('Ctrl Pts',(-51.4727955401375,2.45219266563987,4.89507336172223));
#31885=CARTESIAN_POINT('Ctrl Pts',(-51.3335368960546,-0.194783724789619,
5.47147616156898));
#31886=CARTESIAN_POINT('Ctrl Pts',(-51.1942782519718,-2.79407156101991,
4.70830714779317));
#31887=CARTESIAN_POINT('Ctrl Pts',(-51.055019607889,-4.7092918078351,2.79241163776362));
#31888=CARTESIAN_POINT('Ctrl Pts',(-50.9157609638061,-5.47154448582322,
0.192854934388569));
#31889=CARTESIAN_POINT('Ctrl Pts',(-50.7765023197233,-4.89420862248269,
-2.45391810084947));
#31890=CARTESIAN_POINT('Ctrl Pts',(-50.6372436756404,-3.11863233424258,
-4.49990271560145));
#31891=CARTESIAN_POINT('Ctrl Pts',(-50.4979850315576,-0.579526817574764,
-5.44418412195733));
#31892=CARTESIAN_POINT('Ctrl Pts',(-50.3587263874748,2.10146322296508,-5.05557557638946));
#31893=CARTESIAN_POINT('Ctrl Pts',(-50.2194677433919,4.26795574624971,-3.42921942052629));
#31894=CARTESIAN_POINT('Ctrl Pts',(-50.0802090993091,5.38953222665332,-0.963293550235825));
#31895=CARTESIAN_POINT('Ctrl Pts',(-49.9409504552262,5.19159908182171,1.73847377308041));
#31896=CARTESIAN_POINT('Ctrl Pts',(-49.8016918111434,3.72261593288249,4.01461364296864));
#31897=CARTESIAN_POINT('Ctrl Pts',(-49.6624331670606,1.34223132127078,5.30786276822039));
#31898=CARTESIAN_POINT('Ctrl Pts',(-49.5231745229777,-1.36676940640204,
5.30159725703339));
#31899=CARTESIAN_POINT('Ctrl Pts',(-49.383915878895,-3.74114640211058,3.99735108340956));
#31900=CARTESIAN_POINT('Ctrl Pts',(-49.244657234812,-5.1995851532,1.71444052701824));
#31901=CARTESIAN_POINT('Ctrl Pts',(-49.1053985907293,-5.38501868447694,
-0.988213465752643));
#31902=CARTESIAN_POINT('Ctrl Pts',(-48.9661399466464,-4.25204763305208,
-3.44892490673787));
#31903=CARTESIAN_POINT('Ctrl Pts',(-48.8268813025636,-2.07805529391247,
-5.06524217402316));
#31904=CARTESIAN_POINT('Ctrl Pts',(-48.6876226584808,0.604703640689364,
-5.44144517504289));
#31905=CARTESIAN_POINT('Ctrl Pts',(-48.5483640143978,3.1394140544273,-4.48542879565877));
#31906=CARTESIAN_POINT('Ctrl Pts',(-48.4091053703151,4.90550728800826,-2.43125283205151));
#31907=CARTESIAN_POINT('Ctrl Pts',(-48.2698467262322,5.47059386442934,0.218162454443064));
#31908=CARTESIAN_POINT('Ctrl Pts',(-48.1305880821494,4.6963246384732,2.8141654137826));
#31909=CARTESIAN_POINT('Ctrl Pts',(-47.9913294380664,2.77226257278806,4.72118124133983));
#31910=CARTESIAN_POINT('Ctrl Pts',(-47.8520707939838,0.169472373632881,
5.47231863113212));
#31911=CARTESIAN_POINT('Ctrl Pts',(-47.7128121499008,-2.47480944646745,
4.88367794697152));
#31912=CARTESIAN_POINT('Ctrl Pts',(-47.5735535058181,-4.51318805495189,
3.09937504453724));
#31913=CARTESIAN_POINT('Ctrl Pts',(-47.4342948617351,-5.44661082894759,
0.55625764179145));
#31914=CARTESIAN_POINT('Ctrl Pts',(-47.2950362176524,-5.04654952464708,
-2.12304733375045));
#31915=CARTESIAN_POINT('Ctrl Pts',(-47.1557775735694,-3.41095044230588,
-4.28257039243885));
#31916=CARTESIAN_POINT('Ctrl Pts',(-47.0165189294868,-0.940254407103962,
-5.39359933031572));
#31917=CARTESIAN_POINT('Ctrl Pts',(-46.8772602854037,1.76064244853427,-5.1841229011743));
#31918=CARTESIAN_POINT('Ctrl Pts',(-46.7380016413211,4.03048433321423,-3.70542684798596));
#31919=CARTESIAN_POINT('Ctrl Pts',(-46.5987429972381,5.31354988028646,-1.31953770532269));
#31920=CARTESIAN_POINT('Ctrl Pts',(-46.4594843531554,5.29570842534992,1.38941151562037));
#31921=CARTESIAN_POINT('Ctrl Pts',(-46.3202257090724,3.98132806020307,3.75819357711923));
#31922=CARTESIAN_POINT('Ctrl Pts',(-46.1809670649897,1.69220620066887,5.20686376434782));
#31923=CARTESIAN_POINT('Ctrl Pts',(-46.0417084209068,-1.01121550452221,
5.38074672229371));
#31924=CARTESIAN_POINT('Ctrl Pts',(-45.902449776824,-3.46706310953342,4.23727099446955));
#31925=CARTESIAN_POINT('Ctrl Pts',(-45.7631911327411,-5.07407579679372,
2.05639171717179));
#31926=CARTESIAN_POINT('Ctrl Pts',(-45.6239324886583,-5.43881149757799,
-0.627950300480917));
#31927=CARTESIAN_POINT('Ctrl Pts',(-45.4846738445755,-4.47197261654545,
-3.15855235874414));
#31928=CARTESIAN_POINT('Ctrl Pts',(-45.3454152004926,-2.41026860377883,
-4.915851639716));
#31929=CARTESIAN_POINT('Ctrl Pts',(-45.2061565564098,0.241537200449422,
-5.46961167422877));
#31930=CARTESIAN_POINT('Ctrl Pts',(-45.066897912327,2.8342078798761,-4.68425637425076));
#31931=CARTESIAN_POINT('Ctrl Pts',(-44.9276392682441,4.73298446606043,-2.75206288628934));
#31932=CARTESIAN_POINT('Ctrl Pts',(-44.7883806241613,5.47299285188585,-0.146086718311155));
#31933=CARTESIAN_POINT('Ctrl Pts',(-44.6491219800784,4.8730580954859,2.49565560205727));
#31934=CARTESIAN_POINT('Ctrl Pts',(-44.5098633359956,3.08006116023398,4.52639098347444));
#31935=CARTESIAN_POINT('Ctrl Pts',(-44.3706046919128,0.532978308741886,
5.44893808080723));
#31936=CARTESIAN_POINT('Ctrl Pts',(-44.2313460478299,-2.14459267768491,
5.03743132289471));
#31937=CARTESIAN_POINT('Ctrl Pts',(-44.0920874037471,-4.29710683887934,
3.39261918011984));
#31938=CARTESIAN_POINT('Ctrl Pts',(-43.9528287596642,-5.39756794683762,
0.917198094923704));
#31939=CARTESIAN_POINT('Ctrl Pts',(-43.8135701155814,-5.17655205842662,
-1.78277897465157));
#31940=CARTESIAN_POINT('Ctrl Pts',(-43.6743114714986,-3.68817010198369,
-4.0462814268034));
#31941=CARTESIAN_POINT('Ctrl Pts',(-43.5350528274157,-1.296819994612,-5.31913996691524));
#31942=CARTESIAN_POINT('Ctrl Pts',(-43.395794183333,1.41202825418013,-5.28972289401417));
#31943=CARTESIAN_POINT('Ctrl Pts',(-43.25653553925,3.77517212750151,-3.96523233793384));
#31944=CARTESIAN_POINT('Ctrl Pts',(-43.1172768951672,5.21404729814717,-1.66994097462899));
#31945=CARTESIAN_POINT('Ctrl Pts',(-42.9780182510844,5.37637650765863,1.03419907849356));
#31946=CARTESIAN_POINT('Ctrl Pts',(-42.8387596070015,4.22241698330551,3.48513800374586));
#31947=CARTESIAN_POINT('Ctrl Pts',(-42.6995009629187,2.03469059071199,5.08281676692449));
#31948=CARTESIAN_POINT('Ctrl Pts',(-42.5602423188359,-0.651185493897992,
5.43607850739827));
#31949=CARTESIAN_POINT('Ctrl Pts',(-42.420983674753,-3.17763298788509,4.45843477919831));
#31950=CARTESIAN_POINT('Ctrl Pts',(-42.2817250306702,-4.92610622795756,
2.389240363994));
#31951=CARTESIAN_POINT('Ctrl Pts',(-42.1424663865873,-5.46852960890205,
-0.264907535985755));
#31952=CARTESIAN_POINT('Ctrl Pts',(-42.0032077425046,-4.6721025754924,-2.85419859332491));
#31953=CARTESIAN_POINT('Ctrl Pts',(-41.8639490984217,-2.73181294711378,
-4.74470126647001));
#31954=CARTESIAN_POINT('Ctrl Pts',(-41.7246904543388,-0.122698395445459,
-5.47356713577313));
#31955=CARTESIAN_POINT('Ctrl Pts',(-41.585431810256,2.51645618696809,-4.86234926194433));
#31956=CARTESIAN_POINT('Ctrl Pts',(-41.4461731661731,4.5395112600836,-3.06069103400435));
#31957=CARTESIAN_POINT('Ctrl Pts',(-41.3069145220904,5.45116583504063,-0.509689243506713));
#31958=CARTESIAN_POINT('Ctrl Pts',(-41.1676558780075,5.02822113763075,2.16609886135048));
#31959=CARTESIAN_POINT('Ctrl Pts',(-41.0283972339246,3.37422596869697,4.31156482013568));
#31960=CARTESIAN_POINT('Ctrl Pts',(-40.8891385898418,0.894125034703335,
5.40143800375207));
#31961=CARTESIAN_POINT('Ctrl Pts',(-40.7498799457589,-1.80488294721927,
5.1688866918223));
#31962=CARTESIAN_POINT('Ctrl Pts',(-40.6106213016762,-4.06200463528118,
3.6708460099839));
#31963=CARTESIAN_POINT('Ctrl Pts',(-40.4713626575933,-5.32463292603174,
1.27407860396417));
#31964=CARTESIAN_POINT('Ctrl Pts',(-40.3321040135104,-5.28364077232195,
-1.4346192090996));
#31965=CARTESIAN_POINT('Ctrl Pts',(-40.1928453694276,-3.94906421050984,
-3.79208174322904));
#31966=CARTESIAN_POINT('Ctrl Pts',(-40.0535867253448,-1.64764525546177,
-5.22113562342665));
#31967=CARTESIAN_POINT('Ctrl Pts',(-39.9143280812619,1.05716376798652,-5.37190812037186));
#31968=CARTESIAN_POINT('Ctrl Pts',(-39.7750694371792,3.50314925932756,-4.20748587079426));
#31969=CARTESIAN_POINT('Ctrl Pts',(-39.6358107930962,5.09146492480532,-2.01295231079566));
#31970=CARTESIAN_POINT('Ctrl Pts',(-39.4965521490135,5.43324625440816,0.674408796665931));
#31971=CARTESIAN_POINT('Ctrl Pts',(-39.3572935049306,4.44481553081827,3.1966555934378));
#31972=CARTESIAN_POINT('Ctrl Pts',(-39.2180348608478,2.36816849667272,4.93627086548413));
#31973=CARTESIAN_POINT('Ctrl Pts',(-39.0787762167649,-0.288273034309676,
5.46734768820773));
#31974=CARTESIAN_POINT('Ctrl Pts',(-38.9395175726821,-2.87413718909858,
4.6598634641265));
#31975=CARTESIAN_POINT('Ctrl Pts',(-38.8002589285993,-4.75633142861974,
2.71151312502534));
#31976=CARTESIAN_POINT('Ctrl Pts',(-38.6610002845164,-5.47404147230753,
0.0993078321067214));
#31977=CARTESIAN_POINT('Ctrl Pts',(-38.5217416404335,-4.85155164189017,
-2.53721082138112));
#31978=CARTESIAN_POINT('Ctrl Pts',(-38.3824829963508,-3.04126501954696,
-4.55254864520309));
#31979=CARTESIAN_POINT('Ctrl Pts',(-38.2432243522678,-0.486390871344371,
-5.45329405096895));
#31980=CARTESIAN_POINT('Ctrl Pts',(-38.1039657081851,2.18756549204408,-5.01891913703325));
#31981=CARTESIAN_POINT('Ctrl Pts',(-37.9647070641022,4.32594407220496,-3.35577114389752));
#31982=CARTESIAN_POINT('Ctrl Pts',(-37.8254484200194,5.40520943039183,-0.871035647757145));
#31983=CARTESIAN_POINT('Ctrl Pts',(-37.6861897759365,5.16112694133097,1.82695396261872));
#31984=CARTESIAN_POINT('Ctrl Pts',(-37.5469311318537,3.65345488832461,4.0776536715417));
#31985=CARTESIAN_POINT('Ctrl Pts',(-37.4076724877709,1.25131394863708,5.33002865733449));
#31986=CARTESIAN_POINT('Ctrl Pts',(-37.268413843688,-1.45718396786787,5.27746217133286));
#31987=CARTESIAN_POINT('Ctrl Pts',(-37.1291551996052,-3.80892211553217,
3.93282397316106));
#31988=CARTESIAN_POINT('Ctrl Pts',(-36.9898965555224,-5.22812861075348,
1.62531945028708));
#31989=CARTESIAN_POINT('Ctrl Pts',(-36.8506379114395,-5.36734164202615,
-1.08010915366577));
#31990=CARTESIAN_POINT('Ctrl Pts',(-36.7113792673567,-4.19247792957796,
-3.52109654739291));
#31991=CARTESIAN_POINT('Ctrl Pts',(-36.5721206232738,-1.99117727436389,
-5.10002011252087));
#31992=CARTESIAN_POINT('Ctrl Pts',(-36.432861979191,0.697619784727175,-5.43031479032456));
#31993=CARTESIAN_POINT('Ctrl Pts',(-36.2936033351082,3.21561982804948,-4.43111512009288));
#31994=CARTESIAN_POINT('Ctrl Pts',(-36.1543446910253,4.94634536668937,-2.34705338658735));
#31995=CARTESIAN_POINT('Ctrl Pts',(-36.0150860469425,5.46606593372767,0.311633268767087));
#31996=CARTESIAN_POINT('Ctrl Pts',(-35.8758274028597,4.6475392636393,2.89402330311827));
#31997=CARTESIAN_POINT('Ctrl Pts',(-35.7365687587768,2.6911637906988,4.76787474014284));
#31998=CARTESIAN_POINT('Ctrl Pts',(-35.597310114694,0.0759154554066592,
5.47441585282768));
#31999=CARTESIAN_POINT('Ctrl Pts',(-35.4580514706111,-2.55791912631663,
4.84066543248798));
#32000=CARTESIAN_POINT('Ctrl Pts',(-35.3187928265284,-4.56550290077017,
3.02178347158093));
#32001=CARTESIAN_POINT('Ctrl Pts',(-35.1795341824454,-5.45532268973101,
0.463083617683259));
#32002=CARTESIAN_POINT('Ctrl Pts',(-35.0402755383627,-5.00952549095672,
-2.208992177785));
#32003=CARTESIAN_POINT('Ctrl Pts',(-34.9010168942798,-3.33725504270655,
-4.34024433252211));
#32004=CARTESIAN_POINT('Ctrl Pts',(-34.761758250197,-0.847930355697263,
-5.40888215789063));
#32005=CARTESIAN_POINT('Ctrl Pts',(-34.6224996061141,1.84899161783318,-5.15327294864565));
#32006=CARTESIAN_POINT('Ctrl Pts',(-34.4832409620313,4.09322824983354,-3.63599705456774));
#32007=CARTESIAN_POINT('Ctrl Pts',(-34.3439823179484,5.33532706229741,-1.22852644431343));
#32008=CARTESIAN_POINT('Ctrl Pts',(-34.2047236738656,5.27118720386816,1.47972211845237));
#32009=CARTESIAN_POINT('Ctrl Pts',(-34.0654650297827,3.91651192243436,3.82569293690568));
#32010=CARTESIAN_POINT('Ctrl Pts',(-33.9262063856999,1.60296396677416,5.23502613243565));
#32011=CARTESIAN_POINT('Ctrl Pts',(-33.7869477416171,-1.10303481654853,
5.36267715600542));
#32012=CARTESIAN_POINT('Ctrl Pts',(-33.6476890975343,-3.53897954022436,
4.17739343370168));
#32013=CARTESIAN_POINT('Ctrl Pts',(-33.5084304534514,-5.10848217385333,
1.96936587902892));
#32014=CARTESIAN_POINT('Ctrl Pts',(-33.3691718093686,-5.42728416867607,
-0.720818034248989));
#32015=CARTESIAN_POINT('Ctrl Pts',(-33.2299131652857,-4.4173337971916,-3.23452534543313));
#32016=CARTESIAN_POINT('Ctrl Pts',(-33.0906545212029,-2.32589541929987,
-4.95632954761288));
#32017=CARTESIAN_POINT('Ctrl Pts',(-32.9513958771201,0.334987812800003,
-5.46468436886669));
#32018=CARTESIAN_POINT('Ctrl Pts',(-32.8121372330372,2.91385657226341,-4.63513019907076));
#32019=CARTESIAN_POINT('Ctrl Pts',(-32.6728785889544,4.77933099025839,-2.67076531571315));
#32020=CARTESIAN_POINT('Ctrl Pts',(-32.5336199448715,5.47469027049736,-0.052521692490149));
#32021=CARTESIAN_POINT('Ctrl Pts',(-32.3943613007888,4.82969083251998,2.57858072364102));
#32022=CARTESIAN_POINT('Ctrl Pts',(-32.2551026567059,3.00224674583928,4.57837379024015));
#32023=CARTESIAN_POINT('Ctrl Pts',(-32.115844012623,0.439767908113807,5.45725171428383));
#32024=CARTESIAN_POINT('Ctrl Pts',(-31.9765853685402,-2.23037852732192,
5.0000403709292));
#32025=CARTESIAN_POINT('Ctrl Pts',(-31.8373267244574,-4.35446533996426,
3.31867800322816));
#32026=CARTESIAN_POINT('Ctrl Pts',(-31.6980680803745,-5.41245611918446,
0.824809580426464));
#32027=CARTESIAN_POINT('Ctrl Pts',(-31.5588094362917,-5.14532485718034,
-1.87099551045498));
#32028=CARTESIAN_POINT('Ctrl Pts',(-31.4195507922088,-3.61847282749334,
-4.10872808576484));
#32029=CARTESIAN_POINT('Ctrl Pts',(-31.280292148126,-1.20571650709311,-5.34052804417164));
#32030=CARTESIAN_POINT('Ctrl Pts',(-31.1410335040432,1.50223324930637,-5.26481598450876));
#32031=CARTESIAN_POINT('Ctrl Pts',(-31.0017748599604,3.8423939011143,-3.90012835618781));
#32032=CARTESIAN_POINT('Ctrl Pts',(-30.8625162158775,5.24182806252442,-1.58057921313423));
#32033=CARTESIAN_POINT('Ctrl Pts',(-30.7232575717947,5.35791474748316,1.12594033801213));
#32034=CARTESIAN_POINT('Ctrl Pts',(-30.5839989277118,4.16223265860835,3.55679791127844));
#32035=CARTESIAN_POINT('Ctrl Pts',(-30.444740283629,1.94751852306694,5.11685095428542));
#32036=CARTESIAN_POINT('Ctrl Pts',(-30.3054816395461,-0.74400312163121,
5.42415444480183));
#32037=CARTESIAN_POINT('Ctrl Pts',(-30.1662229954633,-3.25337180037391,
4.40347181376155));
#32038=CARTESIAN_POINT('Ctrl Pts',(-30.0269643513805,-4.96622322594347,
2.30469498115482));
#32039=CARTESIAN_POINT('Ctrl Pts',(-29.8877057072976,-5.4632030188522,-0.358336239954459));
#32040=CARTESIAN_POINT('Ctrl Pts',(-29.7484470632148,-4.62263649701039,
-2.93363663437857));
#32041=CARTESIAN_POINT('Ctrl Pts',(-29.6091884191319,-2.6503180725445,-4.79069996977524));
#32042=CARTESIAN_POINT('Ctrl Pts',(-29.4699297750492,-0.0291269705273693,
-5.47486472030574));
#32043=CARTESIAN_POINT('Ctrl Pts',(-29.3306711309663,2.59919523607336,-4.81862804238241));
#32044=CARTESIAN_POINT('Ctrl Pts',(-29.1914124868835,4.59116107859052,-2.98265519906275));
#32045=CARTESIAN_POINT('Ctrl Pts',(-29.0521538428006,5.45908108940342,-0.416444168380981));
#32046=CARTESIAN_POINT('Ctrl Pts',(-28.9128951987178,4.99046395014899,2.25172415014003));
#32047=CARTESIAN_POINT('Ctrl Pts',(-28.7736365546349,3.30004036467915,4.36860683485581));
#32048=CARTESIAN_POINT('Ctrl Pts',(-28.6343779105521,0.801673744130189,
5.41593124901275));
#32049=CARTESIAN_POINT('Ctrl Pts',(-28.4951192664693,-1.89296523869295,
5.13728281206716));
#32050=CARTESIAN_POINT('Ctrl Pts',(-28.3558606223864,-4.12415289630857,
3.60088252709389));
#32051=CARTESIAN_POINT('Ctrl Pts',(-28.2166019783036,-5.34563150798721,
1.18288455348559));
#32052=CARTESIAN_POINT('Ctrl Pts',(-28.0773433342207,-5.25834862959317,
-1.52471694937658));
#32053=CARTESIAN_POINT('Ctrl Pts',(-27.9380846901379,-3.8836735735854,-3.85902470319832));
#32054=CARTESIAN_POINT('Ctrl Pts',(-27.7988260460551,-1.55816559811303,
-5.24853427681649));
#32055=CARTESIAN_POINT('Ctrl Pts',(-27.6595674019722,1.14882529980163,-5.35305450342104));
#32056=CARTESIAN_POINT('Ctrl Pts',(-27.5203087578894,3.57455133519163,-4.14699588113375));
#32057=CARTESIAN_POINT('Ctrl Pts',(-27.3810501138065,5.12512630100326,-1.92563560541065));
#32058=CARTESIAN_POINT('Ctrl Pts',(-27.2417914697237,5.42092567585061,0.767174623514176));
#32059=CARTESIAN_POINT('Ctrl Pts',(-27.1025328256409,4.38952942292247,3.27215884873556));
#32060=CARTESIAN_POINT('Ctrl Pts',(-26.963274181558,2.28345245927227,4.97602622102256));
#32061=CARTESIAN_POINT('Ctrl Pts',(-26.8240155374752,-0.381678123888043,
5.46162191073365));
#32062=CARTESIAN_POINT('Ctrl Pts',(-26.6847568933923,-2.95336312827968,
4.61005838559325));
#32063=CARTESIAN_POINT('Ctrl Pts',(-26.5454982493096,-4.8019814710958,2.62982243455963));
#32064=CARTESIAN_POINT('Ctrl Pts',(-26.4062396052267,-5.47493919906733,
0.00573171670601601));
#32065=CARTESIAN_POINT('Ctrl Pts',(-26.2669809611439,-4.80747726408187,
-2.61976228719256));
#32066=CARTESIAN_POINT('Ctrl Pts',(-26.127722317061,-2.96300918899314,-4.60386453232529));
#32067=CARTESIAN_POINT('Ctrl Pts',(-25.9884636729782,-0.393112824376433,
-5.4608107816854));
#32068=CARTESIAN_POINT('Ctrl Pts',(-25.8492050288953,2.27302865646815,-4.98079640348159));
#32069=CARTESIAN_POINT('Ctrl Pts',(-25.7099463848125,4.382668558973,-3.28134246738283));
#32070=CARTESIAN_POINT('Ctrl Pts',(-25.5706877407296,5.41930748391964,-0.778523269268893));
#32071=CARTESIAN_POINT('Ctrl Pts',(-25.4314290966468,5.12914696015394,1.91490040137972));
#32072=CARTESIAN_POINT('Ctrl Pts',(-25.292170452564,3.58322647456839,4.13950239980757));
#32073=CARTESIAN_POINT('Ctrl Pts',(-25.1529118084811,1.16003100040254,5.35063736055488));
#32074=CARTESIAN_POINT('Ctrl Pts',(-25.0136531643983,-1.54717280811051,
5.2517852572153));
#32075=CARTESIAN_POINT('Ctrl Pts',(-24.8743945203155,-3.87558503947927,
3.86714787509153));
#32076=CARTESIAN_POINT('Ctrl Pts',(-24.7351358762327,-5.25514465285639,
1.53572353098318));
#32077=CARTESIAN_POINT('Ctrl Pts',(-24.5958772321498,-5.34809651256708,
-1.17168928403761));
#32078=CARTESIAN_POINT('Ctrl Pts',(-24.456618588067,-4.13168337950149,-3.59223948778637));
#32079=CARTESIAN_POINT('Ctrl Pts',(-24.3173599439841,-1.90371752564225,
-5.13330806289892));
#32080=CARTESIAN_POINT('Ctrl Pts',(-24.1781012999013,0.790332116786058,
-5.41759792077973));
#32081=CARTESIAN_POINT('Ctrl Pts',(-24.0388426558185,3.29088614746639,-4.37550687926259));
#32082=CARTESIAN_POINT('Ctrl Pts',(-23.8995840117356,4.98573835384737,-2.26216824154082));
#32083=CARTESIAN_POINT('Ctrl Pts',(-23.7603253676528,5.45994107338208,0.405013038377822));
#32084=CARTESIAN_POINT('Ctrl Pts',(-23.62106672357,4.59739609449573,2.97303569376085));
#32085=CARTESIAN_POINT('Ctrl Pts',(-23.4818080794871,2.60927877600901,4.81317528821976));
#32086=CARTESIAN_POINT('Ctrl Pts',(-23.3425494354043,-0.0176636417764714,
5.47491370542219));
#32087=CARTESIAN_POINT('Ctrl Pts',(-23.2032907913214,-2.64028150144438,
4.79623870123154));
#32088=CARTESIAN_POINT('Ctrl Pts',(-23.0640321472386,-4.61648391947948,
2.94330907436644));
#32089=CARTESIAN_POINT('Ctrl Pts',(-22.9247735031557,-5.46244075954554,
0.369774302130467));
#32090=CARTESIAN_POINT('Ctrl Pts',(-22.7855148590729,-4.97103790745645,
-2.29429165728589));
#32091=CARTESIAN_POINT('Ctrl Pts',(-22.6462562149901,-3.26258465276295,
-4.39665025554866));
#32092=CARTESIAN_POINT('Ctrl Pts',(-22.5069975709072,-0.755358578570335,
-5.42258476225506));
#32093=CARTESIAN_POINT('Ctrl Pts',(-22.3677389268244,1.93680059797925,-5.12091745000131));
#32094=CARTESIAN_POINT('Ctrl Pts',(-22.2284802827416,4.15477631597997,-3.5655049923163));
#32095=CARTESIAN_POINT('Ctrl Pts',(-22.0892216386588,5.35554551046774,-1.13715626514974));
#32096=CARTESIAN_POINT('Ctrl Pts',(-21.9499629945759,5.24512598722233,1.5696004154642));
#32097=CARTESIAN_POINT('Ctrl Pts',(-21.8107043504931,3.85055156246548,3.89207460756537));
#32098=CARTESIAN_POINT('Ctrl Pts',(-21.6714457064102,1.51325342153693,5.26165906993862));
#32099=CARTESIAN_POINT('Ctrl Pts',(-21.5321870623274,-1.19453187322356,
5.34304086545422));
#32100=CARTESIAN_POINT('Ctrl Pts',(-21.3929284182445,-3.60986204607684,
4.11629543331799));
#32101=CARTESIAN_POINT('Ctrl Pts',(-21.2536697741617,-5.14139609057341,
1.88176468398599));
#32102=CARTESIAN_POINT('Ctrl Pts',(-21.1144111300789,-5.41417124035404,
-0.81347517859106));
#32103=CARTESIAN_POINT('Ctrl Pts',(-20.975152485996,-4.36140443883345,-3.30955335460612));
#32104=CARTESIAN_POINT('Ctrl Pts',(-20.8358938419132,-2.24084271661005,
-4.99535944707448));
#32105=CARTESIAN_POINT('Ctrl Pts',(-20.6966351978304,0.42834055732842,-5.45816053748953));
#32106=CARTESIAN_POINT('Ctrl Pts',(-20.5573765537475,2.99265397160103,-4.58464985493124));
#32107=CARTESIAN_POINT('Ctrl Pts',(-20.4181179096647,4.82428121674802,-2.58868747201988));
#32108=CARTESIAN_POINT('Ctrl Pts',(-20.2788592655819,5.4747882398358,0.0410586777207554));
#32109=CARTESIAN_POINT('Ctrl Pts',(-20.139600621499,4.78491255904768,2.66075250414775));
#32110=CARTESIAN_POINT('Ctrl Pts',(-20.0003419774162,2.92355521490692,4.629019009623));
#32111=CARTESIAN_POINT('Ctrl Pts',(-19.8610833333333,0.346429027804539,
5.46397099322049));
#32112=CARTESIAN_POINT('Ctrl Pts',(-19.7218246892505,-2.31551276433093,
4.96118864026364));
#32113=CARTESIAN_POINT('Ctrl Pts',(-19.5825660451676,-4.4105516692771,3.24376726333712));
#32114=CARTESIAN_POINT('Ctrl Pts',(-19.4433074010849,-5.42576302417591,
0.732180095021679));
#32115=CARTESIAN_POINT('Ctrl Pts',(-19.304048757002,-5.11259443188014,-1.95866542859384));
#32116=CARTESIAN_POINT('Ctrl Pts',(-19.1647901129191,-3.54771840393207,
-4.16997436592388));
#32117=CARTESIAN_POINT('Ctrl Pts',(-19.0255314688363,-1.11426076542012,
-5.36035586810296));
#32118=CARTESIAN_POINT('Ctrl Pts',(-18.8862728247535,1.59199936190943,-5.23837094121259));
#32119=CARTESIAN_POINT('Ctrl Pts',(-18.7470141806706,3.90849310635719,-3.83388493875586));
#32120=CARTESIAN_POINT('Ctrl Pts',(-18.6077555365878,5.26807740910997,-1.49075568007831));
#32121=CARTESIAN_POINT('Ctrl Pts',(-18.468496892505,5.33788765439853,1.21735265025395));
#32122=CARTESIAN_POINT('Ctrl Pts',(-18.3292382484221,4.10083232356702,3.62741868827523));
#32123=CARTESIAN_POINT('Ctrl Pts',(-18.1899796043393,1.85977748130069,5.1493902363394));
#32124=CARTESIAN_POINT('Ctrl Pts',(-18.0507209602565,-0.836603386336836,
5.41064569714468));
#32125=CARTESIAN_POINT('Ctrl Pts',(-17.9114623161736,-3.32816012929122,
4.34722235914576));
#32126=CARTESIAN_POINT('Ctrl Pts',(-17.7722036720908,-5.00488932502251,
2.21947627388452));
#32127=CARTESIAN_POINT('Ctrl Pts',(-17.6329450280079,-5.45628033556868,
-0.451660254778956));
#32128=CARTESIAN_POINT('Ctrl Pts',(-17.4936863839251,-4.5718198996462,-3.01221760357043));
#32129=CARTESIAN_POINT('Ctrl Pts',(-17.3544277398423,-2.56804889858935,
-4.8352990538864));
#32130=CARTESIAN_POINT('Ctrl Pts',(-17.2151690957594,0.064452963933669,
-5.47456280459917));
#32131=CARTESIAN_POINT('Ctrl Pts',(-17.0759104516766,2.68117492150221,-4.77349904434557));
#32132=CARTESIAN_POINT('Ctrl Pts',(-16.9366518075937,4.641469573865,-2.90374797132014));
#32133=CARTESIAN_POINT('Ctrl Pts',(-16.7973931635109,5.46540145476815,-0.323077427683596));
#32134=CARTESIAN_POINT('Ctrl Pts',(-16.6581345194281,4.95124878175094,2.33669159010563));
#32135=CARTESIAN_POINT('Ctrl Pts',(-16.5188758753452,3.22489064271104,4.42437254631835));
#32136=CARTESIAN_POINT('Ctrl Pts',(-16.3796172312624,0.708988241862226,
5.42884221164713));
#32137=CARTESIAN_POINT('Ctrl Pts',(-16.2403585871796,-1.98049449397169,
5.10417805776878));
#32138=CARTESIAN_POINT('Ctrl Pts',(-16.1010999430967,-4.185096272123,3.5298670341987));
#32139=CARTESIAN_POINT('Ctrl Pts',(-15.9618412990139,-5.36506834562346,
1.09134491928533));
#32140=CARTESIAN_POINT('Ctrl Pts',(-15.822582654931,-5.23152024253317,-1.61436923844153));
#32141=CARTESIAN_POINT('Ctrl Pts',(-15.6833240108482,-3.81714830829533,
-3.92484023605274));
#32142=CARTESIAN_POINT('Ctrl Pts',(-15.5440653667653,-1.4682307174165,-5.27439955317143));
#32143=CARTESIAN_POINT('Ctrl Pts',(-15.4048067226826,1.24015119842102,-5.33263697349776));
#32144=CARTESIAN_POINT('Ctrl Pts',(-15.2655480785997,3.64490909379705,-4.08529433260519));
#32145=CARTESIAN_POINT('Ctrl Pts',(-15.1262894345169,5.15729035422367,-1.83775631907285));
#32146=CARTESIAN_POINT('Ctrl Pts',(-14.987030790434,5.40702135552813,0.859716317702179));
#32147=CARTESIAN_POINT('Ctrl Pts',(-14.8477721463512,4.33296089916428,3.34670613176209));
#32148=CARTESIAN_POINT('Ctrl Pts',(-14.7085135022683,2.19806930351525,5.01432781367598));
#32149=CARTESIAN_POINT('Ctrl Pts',(-14.5692548581855,-0.474971704911942,
5.45430050195198));
#32150=CARTESIAN_POINT('Ctrl Pts',(-14.4299962141027,-3.03172623243708,
4.55890646291557));
#32151=CARTESIAN_POINT('Ctrl Pts',(-14.2907375700198,-4.84622859844897,
2.54736343257805));
#32152=CARTESIAN_POINT('Ctrl Pts',(-14.151478925937,-5.47423740382875,-0.0878460732350503));
#32153=CARTESIAN_POINT('Ctrl Pts',(-14.0122202818542,-4.76199836553621,
-2.70154838059416));
#32154=CARTESIAN_POINT('Ctrl Pts',(-13.8729616377713,-2.88388770528642,
-4.65383538485821));
#32155=CARTESIAN_POINT('Ctrl Pts',(-13.7337029936885,-0.299719928167668,
-5.46673211806834));
#32156=CARTESIAN_POINT('Ctrl Pts',(-13.5944443496056,2.35782774788484,-4.94121851342003));
#32157=CARTESIAN_POINT('Ctrl Pts',(-13.4551857055228,4.43811263430321,-3.20595513557172));
#32158=CARTESIAN_POINT('Ctrl Pts',(-13.31592706144,5.43182226844271,-0.685783442575275));
#32159=CARTESIAN_POINT('Ctrl Pts',(-13.1766684173571,5.09566848135027,2.00228739551394));
#32160=CARTESIAN_POINT('Ctrl Pts',(-13.0374097732743,3.51195120908233,4.20014175845122));
#32161=CARTESIAN_POINT('Ctrl Pts',(-12.8981511291914,1.06840914518901,5.36968285697927));
#32162=CARTESIAN_POINT('Ctrl Pts',(-12.7588924851086,-1.63670963658612,
5.22457401627795));
#32163=CARTESIAN_POINT('Ctrl Pts',(-12.6196338410258,-3.94111569815331,
3.80034197669499));
#32164=CARTESIAN_POINT('Ctrl Pts',(-12.4803751969429,-5.28062538668073,
1.44567894485724));
#32165=CARTESIAN_POINT('Ctrl Pts',(-12.3411165528601,-5.32728891862932,
-1.26292710142351));
#32166=CARTESIAN_POINT('Ctrl Pts',(-12.2018579087773,-4.06968174415604,
-3.66233294326767));
#32167=CARTESIAN_POINT('Ctrl Pts',(-12.0625992646944,-1.81570159940882,
-5.16509629997009));
#32168=CARTESIAN_POINT('Ctrl Pts',(-11.9233406206116,0.882813550644842,
-5.40329828168483));
#32169=CARTESIAN_POINT('Ctrl Pts',(-11.7840819765288,3.36519102336852,-4.31862031930342));
#32170=CARTESIAN_POINT('Ctrl Pts',(-11.6448233324459,5.02367474068799,-2.17662219639377));
#32171=CARTESIAN_POINT('Ctrl Pts',(-11.5055646883631,5.45222107279121,0.498274482060072));
#32172=CARTESIAN_POINT('Ctrl Pts',(-11.3663060442802,4.5459097805388,3.05117950197334));
#32173=CARTESIAN_POINT('Ctrl Pts',(-11.2270474001974,2.52663145170252,4.85706965086234));
#32174=CARTESIAN_POINT('Ctrl Pts',(-11.0877887561146,-0.111237578466964,
5.47381204346636));
#32175=CARTESIAN_POINT('Ctrl Pts',(-10.9485301120317,-2.72187250940446,
4.75041073262186));
#32176=CARTESIAN_POINT('Ctrl Pts',(-10.8092714679489,-4.66611621680294,
2.86397477945411));
#32177=CARTESIAN_POINT('Ctrl Pts',(-10.670012823866,-5.46796295882303,0.276356955764919));
#32178=CARTESIAN_POINT('Ctrl Pts',(-10.5307541797832,-4.9310980184238,-2.37892085172191));
#32179=CARTESIAN_POINT('Ctrl Pts',(-10.3914955357004,-3.18696108768182,
-4.45177168233753));
#32180=CARTESIAN_POINT('Ctrl Pts',(-10.2522368916175,-0.66256612088064,
-5.43470314014683));
#32181=CARTESIAN_POINT('Ctrl Pts',(-10.1129782475347,2.02404373528209,-5.08706585800951));
#32182=CARTESIAN_POINT('Ctrl Pts',(-9.97371960345187,4.2151105501779,-3.493971255726));
#32183=CARTESIAN_POINT('Ctrl Pts',(-9.83446095936903,5.37419931790948,-1.04545386193834));
#32184=CARTESIAN_POINT('Ctrl Pts',(-9.69520231528619,5.21753238928496,1.65902014840777));
#32185=CARTESIAN_POINT('Ctrl Pts',(-9.55594367120336,3.78346625083831,3.95731919546909));
#32186=CARTESIAN_POINT('Ctrl Pts',(-9.41668502712053,1.4231007741959,5.28675479595409));
#32187=CARTESIAN_POINT('Ctrl Pts',(-9.27742638303767,-1.28567994337311,
5.32184358744868));
#32188=CARTESIAN_POINT('Ctrl Pts',(-9.13816773895486,-3.67968991852724,
4.05399484330575));
#32189=CARTESIAN_POINT('Ctrl Pts',(-8.998909094872,-5.17280793104202,1.7936137250281));
#32190=CARTESIAN_POINT('Ctrl Pts',(-8.85965045078917,-5.39947654359819,
-0.905894663409331));
#32191=CARTESIAN_POINT('Ctrl Pts',(-8.72039180670633,-4.30420088142205,
-3.38361446657658));
#32192=CARTESIAN_POINT('Ctrl Pts',(-8.58113316262349,-2.15513534414405,
-5.03292993538373));
#32193=CARTESIAN_POINT('Ctrl Pts',(-8.44187451854065,0.52156816071472,-5.45004208605669));
#32194=CARTESIAN_POINT('Ctrl Pts',(-8.30261587445781,3.07057705696241,-4.53283008983534));
#32195=CARTESIAN_POINT('Ctrl Pts',(-8.16335723037499,4.86782201316885,-2.50585333452886));
#32196=CARTESIAN_POINT('Ctrl Pts',(-8.02409858629213,5.47328673127907,0.134627052500355));
#32197=CARTESIAN_POINT('Ctrl Pts',(-7.8848399422093,4.73873635719283,2.74214693681418));
#32198=CARTESIAN_POINT('Ctrl Pts',(-7.74558129812648,2.84400955743362,4.67831184545096));
#32199=CARTESIAN_POINT('Ctrl Pts',(-7.60632265404363,0.252988937083455,
5.46909395455718));
#32200=CARTESIAN_POINT('Ctrl Pts',(-7.46706400996079,-2.39997051645686,
4.92088748156248));
#32201=CARTESIAN_POINT('Ctrl Pts',(-7.32780536587795,-4.46534944100724,
3.16790884587246));
#32202=CARTESIAN_POINT('Ctrl Pts',(-7.18854672179511,-5.43748477415477,
0.639336700726373));
#32203=CARTESIAN_POINT('Ctrl Pts',(-7.04928807771227,-5.07837034483033,
-2.04576311600544));
#32204=CARTESIAN_POINT('Ctrl Pts',(-6.91002943362945,-3.47592750244373,
-4.23000237397282));
#32205=CARTESIAN_POINT('Ctrl Pts',(-6.7707707895466,-1.02247948869701,-5.37861764594346));
#32206=CARTESIAN_POINT('Ctrl Pts',(-6.63151214546376,1.68130036651628,-5.21039549013439));
#32207=CARTESIAN_POINT('Ctrl Pts',(-6.49225350138094,3.97345043212405,-3.76652143887618));
#32208=CARTESIAN_POINT('Ctrl Pts',(-6.35299485729809,5.29278766906849,-1.40049661771002));
#32209=CARTESIAN_POINT('Ctrl Pts',(-6.21373621321525,5.31630107938763,1.30840930880301));
#32210=CARTESIAN_POINT('Ctrl Pts',(-6.07447756913241,4.03823391649698,3.69697970263754));
#32211=CARTESIAN_POINT('Ctrl Pts',(-5.93521892504958,1.77149309925507,5.18042510662517));
#32212=CARTESIAN_POINT('Ctrl Pts',(-5.79596028096673,-0.928959234534617,
5.39555621105307));
#32213=CARTESIAN_POINT('Ctrl Pts',(-5.6567016368839,-3.40197612497396,4.28970284881921));
#32214=CARTESIAN_POINT('Ctrl Pts',(-5.51744299280106,-5.04209322876317,
2.13360913911639));
#32215=CARTESIAN_POINT('Ctrl Pts',(-5.37818434871823,-5.44776358153681,
-0.544852315532973));
#32216=CARTESIAN_POINT('Ctrl Pts',(-5.23892570463539,-4.51966762964043,
-3.08991854320483));
#32217=CARTESIAN_POINT('Ctrl Pts',(-5.09966706055256,-2.48502946046558,
-4.87848548903026));
#32218=CARTESIAN_POINT('Ctrl Pts',(-4.96040841646971,0.158014068243348,
-5.47266147685913));
#32219=CARTESIAN_POINT('Ctrl Pts',(-4.82114977238688,2.76237129261238,-4.72697545242317));
#32220=CARTESIAN_POINT('Ctrl Pts',(-4.68189112830404,4.69042204811024,-2.82399240378975));
#32221=CARTESIAN_POINT('Ctrl Pts',(-4.54263248422121,5.47012508461874,-0.229616298823035));
#32222=CARTESIAN_POINT('Ctrl Pts',(-4.40337384013836,4.91058708928048,2.42097635772262));
#32223=CARTESIAN_POINT('Ctrl Pts',(-4.26411519605553,3.14879875803774,4.47884566238253));
#32224=CARTESIAN_POINT('Ctrl Pts',(-4.12485655197269,0.616095606282331,
5.44016711967324));
#32225=CARTESIAN_POINT('Ctrl Pts',(-3.98559790788985,-2.06744514108811,
5.06958210059417));
#32226=CARTESIAN_POINT('Ctrl Pts',(-3.84633926380702,-4.24481695791071,
3.45782027871221));
#32227=CARTESIAN_POINT('Ctrl Pts',(-3.70708061972418,-5.38293776040373,
0.999486444981389));
#32228=CARTESIAN_POINT('Ctrl Pts',(-3.56782197564132,-5.20316344914374,
-1.70354988408383));
#32229=CARTESIAN_POINT('Ctrl Pts',(-3.4285633315585,-3.74950785022513,-3.98950911354476));
#32230=CARTESIAN_POINT('Ctrl Pts',(-3.28930468747566,-1.37786688814311,
-5.29872389589696));
#32231=CARTESIAN_POINT('Ctrl Pts',(-3.15004604339282,1.3311147826584,-5.31066149558737));
#32232=CARTESIAN_POINT('Ctrl Pts',(-3.01078739930999,3.71420197991916,-4.02239925165122));
#32233=CARTESIAN_POINT('Ctrl Pts',(-2.87152875522716,5.18794768756703,-1.7493401257652));
#32234=CARTESIAN_POINT('Ctrl Pts',(-2.73227011114431,5.39153735575714,0.952006842378526));
#32235=CARTESIAN_POINT('Ctrl Pts',(-2.59301146706148,4.27512648599062,3.42027566421813));
#32236=CARTESIAN_POINT('Ctrl Pts',(-2.45375282297864,2.11204397484455,5.05116445166812));
#32237=CARTESIAN_POINT('Ctrl Pts',(-2.3144941788958,-0.568126522254023,
5.44538560441941));
#32238=CARTESIAN_POINT('Ctrl Pts',(-2.17523553481295,-3.10920360575483,
4.50642263331263));
#32239=CARTESIAN_POINT('Ctrl Pts',(-2.03597689073012,-4.8890598871849,2.46416022338722));
#32240=CARTESIAN_POINT('Ctrl Pts',(-1.89671824664729,-5.47193628488737,
-0.181398225237268));
#32241=CARTESIAN_POINT('Ctrl Pts',(-1.75745960256445,-4.71512824620705,
-2.78254515563813));
#32242=CARTESIAN_POINT('Ctrl Pts',(-1.61820095848162,-2.80392365840489,
-4.70244670481565));
#32243=CARTESIAN_POINT('Ctrl Pts',(-1.47894231439878,-0.206239517764929,
-5.47105613283949));
#32244=CARTESIAN_POINT('Ctrl Pts',(-1.33968367031593,2.44193808947732,-4.90019741459951));
#32245=CARTESIAN_POINT('Ctrl Pts',(-1.2004250262331,4.4922599097877,-3.12963042226007));
#32246=CARTESIAN_POINT('Ctrl Pts',(-1.06116638215027,5.44275049879988,-0.592844726594321));
#32247=CARTESIAN_POINT('Ctrl Pts',(-0.92190773806742,5.06070056194062,2.089092271632));
#32248=CARTESIAN_POINT('Ctrl Pts',(-0.782649093984577,3.43965132709995,
4.25954845848455));
#32249=CARTESIAN_POINT('Ctrl Pts',(-0.643390449901751,0.976472396486427,
5.3871704534383));
#32250=CARTESIAN_POINT('Ctrl Pts',(-0.504131805818906,-1.72576292242332,
5.19581519094514));
#32251=CARTESIAN_POINT('Ctrl Pts',(-0.364873161736073,-4.00550542683706,
3.73246718521018));
#32252=CARTESIAN_POINT('Ctrl Pts',(-0.225614517653244,-5.30454291679212,
1.35513103364222));
#32253=CARTESIAN_POINT('Ctrl Pts',(-0.0863558735703945,-5.30496491583615,
-1.35363561368514));
#32254=CARTESIAN_POINT('Ctrl Pts',(0.0529027705124452,-4.00641227436962,
-3.73169439030285));
#32255=CARTESIAN_POINT('Ctrl Pts',(0.145741866567666,-2.48701521175681,
-4.70686214717463));
#32256=CARTESIAN_POINT('Ctrl Pts',(0.192161414595278,-1.65653546761383,
-4.98294756325496));
#32257=CARTESIAN_POINT('Ctrl Pts',(-59.7754114145953,-2.43856727558405,
5.02329722221654));
#32258=CARTESIAN_POINT('Ctrl Pts',(-59.7289918665677,-3.27577186963271,
4.61687497887677));
#32259=CARTESIAN_POINT('Ctrl Pts',(-59.6361527705125,-4.7421817453593,3.37773902727111));
#32260=CARTESIAN_POINT('Ctrl Pts',(-59.4968941264296,-5.7809011470696,0.690247673182852));
#32261=CARTESIAN_POINT('Ctrl Pts',(-59.3576354823468,-5.40421136209148,
-2.16547390737938));
#32262=CARTESIAN_POINT('Ctrl Pts',(-59.2183768382639,-3.70446136576718,
-4.49140083748381));
#32263=CARTESIAN_POINT('Ctrl Pts',(-59.0791181941811,-1.09773232127279,
-5.71751561060345));
#32264=CARTESIAN_POINT('Ctrl Pts',(-58.9398595500983,1.77774111756532,-5.54391865569175));
#32265=CARTESIAN_POINT('Ctrl Pts',(-58.8006009060154,4.21797922743172,-4.01296395592685));
#32266=CARTESIAN_POINT('Ctrl Pts',(-58.6613422619326,5.62553394302333,-1.49954801434181));
#32267=CARTESIAN_POINT('Ctrl Pts',(-58.5220836178498,5.65580069646275,1.38101274096256));
#32268=CARTESIAN_POINT('Ctrl Pts',(-58.3828249737669,4.3013669948914,3.92345586255738));
#32269=CARTESIAN_POINT('Ctrl Pts',(-58.2435663296841,1.89383763972005,5.50532968824863));
#32270=CARTESIAN_POINT('Ctrl Pts',(-58.1043076856012,-0.977356837237599,
5.73934163225416));
#32271=CARTESIAN_POINT('Ctrl Pts',(-57.9650490415184,-3.60926666480663,
4.56820164103017));
#32272=CARTESIAN_POINT('Ctrl Pts',(-57.8257903974356,-5.35752618487369,
2.2786364715673));
#32273=CARTESIAN_POINT('Ctrl Pts',(-57.6865317533527,-5.79411203415328,
-0.568802989310091));
#32274=CARTESIAN_POINT('Ctrl Pts',(-57.54727310927,-4.81213571518974,-3.2769835443839));
#32275=CARTESIAN_POINT('Ctrl Pts',(-57.408014465187,-2.65201272842086,-5.18286596219213));
#32276=CARTESIAN_POINT('Ctrl Pts',(-57.2687558211043,0.157397831715513,
-5.81983652221233));
#32277=CARTESIAN_POINT('Ctrl Pts',(-57.1294971770213,2.92827296154665,-5.03194680231615));
#32278=CARTESIAN_POINT('Ctrl Pts',(-56.9902385329385,4.98222420987256,-3.01209447145306));
#32279=CARTESIAN_POINT('Ctrl Pts',(-56.8509798888557,5.81638633350395,-0.254796384005554));
#32280=CARTESIAN_POINT('Ctrl Pts',(-56.7117212447728,5.2265328970099,2.56488304844114));
#32281=CARTESIAN_POINT('Ctrl Pts',(-56.5724626006901,3.35707667246942,4.75660671004105));
#32282=CARTESIAN_POINT('Ctrl Pts',(-56.4332039566071,0.665713314608688,
5.78377877856199));
#32283=CARTESIAN_POINT('Ctrl Pts',(-56.2939453125244,-2.18863545444221,
5.3949185374159));
#32284=CARTESIAN_POINT('Ctrl Pts',(-56.1546866684414,-4.50714448328554,
3.68522994996149));
#32285=CARTESIAN_POINT('Ctrl Pts',(-56.0154280243587,-5.72217731457325,
1.07329304386676));
#32286=CARTESIAN_POINT('Ctrl Pts',(-55.8761693802758,-5.53625961317535,
-1.80141629640945));
#32287=CARTESIAN_POINT('Ctrl Pts',(-55.7369107361931,-3.99490928048671,
-4.23508807677945));
#32288=CARTESIAN_POINT('Ctrl Pts',(-55.5976520921101,-1.47549238731475,
-5.63189074755655));
#32289=CARTESIAN_POINT('Ctrl Pts',(-55.4583934480274,1.40516669259064,-5.64984758586005));
#32290=CARTESIAN_POINT('Ctrl Pts',(-55.3191348039445,3.94180130099076,-4.28456225079436));
#32291=CARTESIAN_POINT('Ctrl Pts',(-55.1798761598616,5.51337168142342,-1.87029513176393));
#32292=CARTESIAN_POINT('Ctrl Pts',(-55.0406175157788,5.73511304234294,1.00187303036342));
#32293=CARTESIAN_POINT('Ctrl Pts',(-54.9013588716959,4.55273683926334,3.62875439370546));
#32294=CARTESIAN_POINT('Ctrl Pts',(-54.7621002276132,2.25572214290931,5.36721424869647));
#32295=CARTESIAN_POINT('Ctrl Pts',(-54.6228415835303,-0.593557008735543,
5.79162854944988));
#32296=CARTESIAN_POINT('Ctrl Pts',(-54.4835829394474,-3.2975166496668,4.79808869474004));
#32297=CARTESIAN_POINT('Ctrl Pts',(-54.3443242953646,-5.19415113219364,
2.62984128672311));
#32298=CARTESIAN_POINT('Ctrl Pts',(-54.2050656512818,-5.81911079664231,
-0.182265503655628));
#32299=CARTESIAN_POINT('Ctrl Pts',(-54.065807007199,-5.01938787574395,-2.94974855373413));
#32300=CARTESIAN_POINT('Ctrl Pts',(-53.9265483631161,-2.9907771151776,-4.99504989211838));
#32301=CARTESIAN_POINT('Ctrl Pts',(-53.7872897190333,-0.229939692918102,
-5.81742201624076));
#32302=CARTESIAN_POINT('Ctrl Pts',(-53.6480310749504,2.58719345692394,-5.21552501612943));
#32303=CARTESIAN_POINT('Ctrl Pts',(-53.5087724308677,4.7709086170054,-3.33672026780873));
#32304=CARTESIAN_POINT('Ctrl Pts',(-53.3695137867847,5.78657067405063,-0.640992208719566));
#32305=CARTESIAN_POINT('Ctrl Pts',(-53.230255142702,5.38551688630448,2.21166883704392));
#32306=CARTESIAN_POINT('Ctrl Pts',(-53.0909964986191,3.66593654198589,4.52285092033272));
#32307=CARTESIAN_POINT('Ctrl Pts',(-52.9517378545363,1.04883144983671,5.72671142692343));
#32308=CARTESIAN_POINT('Ctrl Pts',(-52.8124792104535,-1.82505718773126,
5.52851132213115));
#32309=CARTESIAN_POINT('Ctrl Pts',(-52.6732205663706,-4.2521203078811,3.97677558641761));
#32310=CARTESIAN_POINT('Ctrl Pts',(-52.5339619222877,-5.63814434746659,
1.45141293040697));
#32311=CARTESIAN_POINT('Ctrl Pts',(-52.3947032782049,-5.64379149679879,
-1.42929658156861));
#32312=CARTESIAN_POINT('Ctrl Pts',(-52.255444634122,-4.26767917431298,-3.96007394407695));
#32313=CARTESIAN_POINT('Ctrl Pts',(-52.1161859900392,-1.84671852156337,
-5.52131341978852));
#32314=CARTESIAN_POINT('Ctrl Pts',(-51.9769273459564,1.02637095458436,-5.73077951425524));
#32315=CARTESIAN_POINT('Ctrl Pts',(-51.8376687018736,3.64817584856774,-4.53718901472586));
#32316=CARTESIAN_POINT('Ctrl Pts',(-51.6984100577907,5.3768043138196,-2.23276656825405));
#32317=CARTESIAN_POINT('Ctrl Pts',(-51.5591514137078,5.78903930618248,0.618300160841148));
#32318=CARTESIAN_POINT('Ctrl Pts',(-51.4198927696251,4.78395406292337,3.3179895571356));
#32319=CARTESIAN_POINT('Ctrl Pts',(-51.2806341255421,2.60762182321943,5.20534144936639));
#32320=CARTESIAN_POINT('Ctrl Pts',(-51.1413754814594,-0.207129846967831,
5.81827881799394));
#32321=CARTESIAN_POINT('Ctrl Pts',(-51.0021168373764,-2.97117028373933,
5.00673729313276));
#32322=CARTESIAN_POINT('Ctrl Pts',(-50.8628581932937,-5.00778436461698,
2.96940514832847));
#32323=CARTESIAN_POINT('Ctrl Pts',(-50.7235995492108,-5.81835147289538,
0.205078802605319));
#32324=CARTESIAN_POINT('Ctrl Pts',(-50.584340905128,-5.20442189971427,-2.60945662297661));
#32325=CARTESIAN_POINT('Ctrl Pts',(-50.4450822610452,-3.31630293464185,
-4.78512340730182));
#32326=CARTESIAN_POINT('Ctrl Pts',(-50.3058236169624,-0.616259398302359,
-5.78925690666997));
#32327=CARTESIAN_POINT('Ctrl Pts',(-50.1665649728795,2.23466183456155,-5.37601689567433));
#32328=CARTESIAN_POINT('Ctrl Pts',(-50.0273063287967,4.53847477011026,-3.64657619397903));
#32329=CARTESIAN_POINT('Ctrl Pts',(-49.8880476847138,5.73114096950406,-1.02435070415067));
#32330=CARTESIAN_POINT('Ctrl Pts',(-49.748789040631,5.52066208045366,1.84866475350808));
#32331=CARTESIAN_POINT('Ctrl Pts',(-49.6095303965482,3.95856927641364,4.26907489525025));
#32332=CARTESIAN_POINT('Ctrl Pts',(-49.4702717524652,1.42730697069471,5.64429499484464));
#32333=CARTESIAN_POINT('Ctrl Pts',(-49.3310131083825,-1.45340037158661,
5.63763235208663));
#32334=CARTESIAN_POINT('Ctrl Pts',(-49.1917544642997,-3.97827427620059,
4.250718169997));
#32335=CARTESIAN_POINT('Ctrl Pts',(-49.0524958202168,-5.52915433895347,
1.8231081902767));
#32336=CARTESIAN_POINT('Ctrl Pts',(-48.913237176134,-5.72634134211583,-1.05085013726839));
#32337=CARTESIAN_POINT('Ctrl Pts',(-48.7739785320511,-4.5215583411029,-3.66753068772775));
#32338=CARTESIAN_POINT('Ctrl Pts',(-48.6347198879683,-2.20977022327436,
-5.38629619847924));
#32339=CARTESIAN_POINT('Ctrl Pts',(-48.4954612438854,0.643032022783838,
-5.7863443550394));
#32340=CARTESIAN_POINT('Ctrl Pts',(-48.3562025998026,3.33840187810475,-4.76973207609072));
#32341=CARTESIAN_POINT('Ctrl Pts',(-48.2169439557197,5.21643671698811,-2.58535474453319));
#32342=CARTESIAN_POINT('Ctrl Pts',(-48.0776853116369,5.81734059755632,0.231990408088362));
#32343=CARTESIAN_POINT('Ctrl Pts',(-47.9384266675541,4.99399528748307,2.99253776016594));
#32344=CARTESIAN_POINT('Ctrl Pts',(-47.7991680234712,2.9479789601321,5.02042739495756));
#32345=CARTESIAN_POINT('Ctrl Pts',(-47.6599093793884,0.18021416755293,5.81917468643407));
#32346=CARTESIAN_POINT('Ctrl Pts',(-47.5206507353056,-2.63167214034327,
5.19322375053906));
#32347=CARTESIAN_POINT('Ctrl Pts',(-47.3813920912227,-4.79925082122997,
3.29582504577313));
#32348=CARTESIAN_POINT('Ctrl Pts',(-47.2421334471399,-5.79183742744024,
0.591515334986651));
#32349=CARTESIAN_POINT('Ctrl Pts',(-47.1028748030571,-5.36641873895901,
-2.25761402714712));
#32350=CARTESIAN_POINT('Ctrl Pts',(-46.9636161589742,-3.62714925947957,
-4.55401574732442));
#32351=CARTESIAN_POINT('Ctrl Pts',(-46.8243575148914,-0.999851253817615,
-5.73546586143282));
#32352=CARTESIAN_POINT('Ctrl Pts',(-46.6850988708086,1.87223856266074,-5.51271203146944));
#32353=CARTESIAN_POINT('Ctrl Pts',(-46.5458402267257,4.28595152929855,-3.94029068292243));
#32354=CARTESIAN_POINT('Ctrl Pts',(-46.4065815826429,5.65034257737858,-1.40317494835275));
#32355=CARTESIAN_POINT('Ctrl Pts',(-46.26732293856,5.63137026419025,1.47747762250932));
#32356=CARTESIAN_POINT('Ctrl Pts',(-46.1280642944772,4.23367954755404,3.9964019650236));
#32357=CARTESIAN_POINT('Ctrl Pts',(-45.9888056503944,1.79946456902883,5.53689429574304));
#32358=CARTESIAN_POINT('Ctrl Pts',(-45.8495470063115,-1.07531013142566,
5.72179860696575));
#32359=CARTESIAN_POINT('Ctrl Pts',(-45.7102883622287,-3.68681855776603,
4.50584510381061));
#32360=CARTESIAN_POINT('Ctrl Pts',(-45.5710297181458,-5.39568972935361,
2.18673352788352));
#32361=CARTESIAN_POINT('Ctrl Pts',(-45.431771074063,-5.78354374523047,-0.667752142959872));
#32362=CARTESIAN_POINT('Ctrl Pts',(-45.2925124299802,-4.7554229939355,-3.35875323984533));
#32363=CARTESIAN_POINT('Ctrl Pts',(-45.1532537858973,-2.56304045726125,
-5.22743673245922));
#32364=CARTESIAN_POINT('Ctrl Pts',(-45.0139951418145,0.256846733063343,
-5.81629615246135));
#32365=CARTESIAN_POINT('Ctrl Pts',(-44.8747364977317,3.01385059284374,-4.98116209146394));
#32366=CARTESIAN_POINT('Ctrl Pts',(-44.7354778536488,5.03297875227833,-2.92649894183081));
#32367=CARTESIAN_POINT('Ctrl Pts',(-44.596219209566,5.81989164182494,-0.155346241789309));
#32368=CARTESIAN_POINT('Ctrl Pts',(-44.4569605654831,5.18193077308208,2.65383960336846));
#32369=CARTESIAN_POINT('Ctrl Pts',(-44.3177019214003,3.27528697512884,4.81329060082324));
#32370=CARTESIAN_POINT('Ctrl Pts',(-44.1784432773175,0.566760470599109,
5.79431218924112));
#32371=CARTESIAN_POINT('Ctrl Pts',(-44.0391846332346,-2.28052499569356,
5.35672259142087));
#32372=CARTESIAN_POINT('Ctrl Pts',(-43.8999259891518,-4.5694735681969,3.60765609322339));
#32373=CARTESIAN_POINT('Ctrl Pts',(-43.7606673450689,-5.73968602373716,
0.975333546197558));
#32374=CARTESIAN_POINT('Ctrl Pts',(-43.6214087009861,-5.50466132034644,
-1.89577818473146));
#32375=CARTESIAN_POINT('Ctrl Pts',(-43.4821500569033,-3.92194013971112,
-4.30274990185865));
#32376=CARTESIAN_POINT('Ctrl Pts',(-43.3428914128205,-1.37901730403188,
-5.65628698463953));
#32377=CARTESIAN_POINT('Ctrl Pts',(-43.2036327687376,1.50152789468607,-5.62500534745538));
#32378=CARTESIAN_POINT('Ctrl Pts',(-43.0643741246547,4.01445667953435,-4.21656361810942));
#32379=CARTESIAN_POINT('Ctrl Pts',(-42.925115480572,5.54453314882563,-1.7757880895523));
#32380=CARTESIAN_POINT('Ctrl Pts',(-42.785856836489,5.71715139175535,1.09975049041664));
#32381=CARTESIAN_POINT('Ctrl Pts',(-42.6465981924063,4.49004958977272,3.70603910648602));
#32382=CARTESIAN_POINT('Ctrl Pts',(-42.5073395483234,2.1636569027317,5.40498473491679));
#32383=CARTESIAN_POINT('Ctrl Pts',(-42.3680809042406,-0.692460069979665,
5.7806375278948));
#32384=CARTESIAN_POINT('Ctrl Pts',(-42.2288222601578,-3.37904327074129,
4.7410270777417));
#32385=CARTESIAN_POINT('Ctrl Pts',(-42.0895636160749,-5.23834129491938,
2.54067936886263));
#32386=CARTESIAN_POINT('Ctrl Pts',(-41.9503049719921,-5.81514550178058,
-0.281698368016173));
#32387=CARTESIAN_POINT('Ctrl Pts',(-41.8110463279093,-4.96823793940958,
-3.03510839260038));
#32388=CARTESIAN_POINT('Ctrl Pts',(-41.6717876838263,-2.90496548564975,
-5.04543820739147));
#32389=CARTESIAN_POINT('Ctrl Pts',(-41.5325290397437,-0.13047547940279,
-5.8205023259764));
#32390=CARTESIAN_POINT('Ctrl Pts',(-41.3932703956606,2.67595860727431,-5.17054317355309));
#32391=CARTESIAN_POINT('Ctrl Pts',(-41.2540117515779,4.82724248971522,-3.2546890977342));
#32392=CARTESIAN_POINT('Ctrl Pts',(-41.1147531074951,5.79668114688347,-0.541995257163577));
#32393=CARTESIAN_POINT('Ctrl Pts',(-40.9754944634122,5.34692863011159,2.30339432184656));
#32394=CARTESIAN_POINT('Ctrl Pts',(-40.8362358193294,3.58809705115569,4.58484795046792));
#32395=CARTESIAN_POINT('Ctrl Pts',(-40.6969771752465,0.950798028983867,
5.7438013793569));
#32396=CARTESIAN_POINT('Ctrl Pts',(-40.5577185311637,-1.91928318988664,
5.49651009409065));
#32397=CARTESIAN_POINT('Ctrl Pts',(-40.4184598870809,-4.31946970619222,
3.90351798186069));
#32398=CARTESIAN_POINT('Ctrl Pts',(-40.279201242998,-5.66212810808261,1.35483447885073));
#32399=CARTESIAN_POINT('Ctrl Pts',(-40.1399425989152,-5.6185377181054,-1.52555074895882));
#32400=CARTESIAN_POINT('Ctrl Pts',(-40.0006839548323,-4.19937069420006,
-4.03243809005368));
#32401=CARTESIAN_POINT('Ctrl Pts',(-39.8614253107495,-1.75207918417979,
-5.55207075871569));
#32402=CARTESIAN_POINT('Ctrl Pts',(-39.7221666666667,1.12417076796024,-5.71239978134284));
#32403=CARTESIAN_POINT('Ctrl Pts',(-39.5829080225839,3.72519198292045,-4.4741720874154));
#32404=CARTESIAN_POINT('Ctrl Pts',(-39.443649378501,5.41418104544193,-2.14054076919809));
#32405=CARTESIAN_POINT('Ctrl Pts',(-39.3043907344182,5.77762575609995,0.717155352676428));
#32406=CARTESIAN_POINT('Ctrl Pts',(-39.1651320903353,4.72654459037877,3.39927160029664));
#32407=CARTESIAN_POINT('Ctrl Pts',(-39.0258734462525,2.51827188765085,5.24915020525126));
#32408=CARTESIAN_POINT('Ctrl Pts',(-38.8866148021696,-0.306544859155955,
5.81388866652493));
#32409=CARTESIAN_POINT('Ctrl Pts',(-38.7473561580868,-3.05631077126836,
4.95522306731501));
#32410=CARTESIAN_POINT('Ctrl Pts',(-38.608097514004,-5.05780553278731,2.88337898478993));
#32411=CARTESIAN_POINT('Ctrl Pts',(-38.4688388699212,-5.8210067277373,0.105602334533653));
#32412=CARTESIAN_POINT('Ctrl Pts',(-38.3295802258383,-5.15906115988973,
-2.69802874816768));
#32413=CARTESIAN_POINT('Ctrl Pts',(-38.1903215817555,-3.23403178970654,
-4.84110623314438));
#32414=CARTESIAN_POINT('Ctrl Pts',(-38.0510629376726,-0.517220146892966,
-5.79894425711007));
#32415=CARTESIAN_POINT('Ctrl Pts',(-37.9118042935898,2.32622158801205,-5.33703703386896));
#32416=CARTESIAN_POINT('Ctrl Pts',(-37.7725456495069,4.60013861340107,-3.56847249042477));
#32417=CARTESIAN_POINT('Ctrl Pts',(-37.6332870054241,5.74781185314564,-0.926245150195311));
#32418=CARTESIAN_POINT('Ctrl Pts',(-37.4940283613413,5.48825850154353,1.9427531489248));
#32419=CARTESIAN_POINT('Ctrl Pts',(-37.3547697172584,3.88502454575981,4.33611063699552));
#32420=CARTESIAN_POINT('Ctrl Pts',(-37.2155110731756,1.33062691438782,5.66786584104888));
#32421=CARTESIAN_POINT('Ctrl Pts',(-37.0762524290928,-1.54954574667018,
5.61196749423928));
#32422=CARTESIAN_POINT('Ctrl Pts',(-36.9369937850099,-4.05034586824098,
4.18210108976877));
#32423=CARTESIAN_POINT('Ctrl Pts',(-36.7977351409272,-5.55950698777649,
1.72833828583595));
#32424=CARTESIAN_POINT('Ctrl Pts',(-36.6584764968442,-5.70754386249259,
-1.1485705181421));
#32425=CARTESIAN_POINT('Ctrl Pts',(-36.5192178527615,-4.4582128866619,-3.74427683733772));
#32426=CARTESIAN_POINT('Ctrl Pts',(-36.3799592086786,-2.11738554938339,
-5.42327849300442));
#32427=CARTESIAN_POINT('Ctrl Pts',(-36.2407005645957,0.741837540114254,
-5.77450848484087));
#32428=CARTESIAN_POINT('Ctrl Pts',(-36.1014419205129,3.41943785914202,-4.71197579629695));
#32429=CARTESIAN_POINT('Ctrl Pts',(-35.96218327643,5.25986326608409,-2.49581842278662));
#32430=CARTESIAN_POINT('Ctrl Pts',(-35.8229246323472,5.81252566964419,0.331385752785651));
#32431=CARTESIAN_POINT('Ctrl Pts',(-35.6836659882644,4.94211771283189,3.0774573416922));
#32432=CARTESIAN_POINT('Ctrl Pts',(-35.5444073441815,2.86173983342087,5.07008050263841));
#32433=CARTESIAN_POINT('Ctrl Pts',(-35.4051487000987,0.0807272613655634,
5.82140483789733));
#32434=CARTESIAN_POINT('Ctrl Pts',(-35.2658900560158,-2.72004962304768,
5.1474849417536));
#32435=CARTESIAN_POINT('Ctrl Pts',(-35.126631411933,-4.85488157795867,3.21331542824843));
#32436=CARTESIAN_POINT('Ctrl Pts',(-34.9873727678502,-5.80110147859658,
0.492435592180922));
#32437=CARTESIAN_POINT('Ctrl Pts',(-34.8481141237674,-5.32704798331352,
-2.34900637736412));
#32438=CARTESIAN_POINT('Ctrl Pts',(-34.7088554796845,-3.5487827693751,-4.61534527778891));
#32439=CARTESIAN_POINT('Ctrl Pts',(-34.5695968356017,-0.901675358167371,
-5.75171737187212));
#32440=CARTESIAN_POINT('Ctrl Pts',(-34.4303381915188,1.96618763328446,-5.47990669337911));
#32441=CARTESIAN_POINT('Ctrl Pts',(-34.2910795474361,4.35267239040516,-3.86646016909869));
#32442=CARTESIAN_POINT('Ctrl Pts',(-34.1518209033531,5.6735000787673,-1.30639505267333));
#32443=CARTESIAN_POINT('Ctrl Pts',(-34.0125622592703,5.60529479582931,1.57351244967139));
#32444=CARTESIAN_POINT('Ctrl Pts',(-33.8733036151875,4.16475512015862,4.06817968710017));
#32445=CARTESIAN_POINT('Ctrl Pts',(-33.7340449711046,1.70456582802962,5.56684170022245));
#32446=CARTESIAN_POINT('Ctrl Pts',(-33.5947863270218,-1.17294929542274,
5.7025837238737));
#32447=CARTESIAN_POINT('Ctrl Pts',(-33.455527682939,-3.76329332124829,4.44217227892728));
#32448=CARTESIAN_POINT('Ctrl Pts',(-33.3162690388561,-5.43227691148481,
2.09419166610201));
#32449=CARTESIAN_POINT('Ctrl Pts',(-33.1770103947733,-5.77128577103893,
-0.766506181596307));
#32450=CARTESIAN_POINT('Ctrl Pts',(-33.0377517506904,-4.69732096152246,
-3.4395416790415));
#32451=CARTESIAN_POINT('Ctrl Pts',(-32.8984931066076,-2.47331938427025,
-5.27048028179739));
#32452=CARTESIAN_POINT('Ctrl Pts',(-32.7592344625248,0.356220595310421,
-5.8110565360267));
#32453=CARTESIAN_POINT('Ctrl Pts',(-32.619975818442,3.09854771773538,-4.92892211526402));
#32454=CARTESIAN_POINT('Ctrl Pts',(-32.4807171743591,5.08226289280382,-2.84004842667364));
#32455=CARTESIAN_POINT('Ctrl Pts',(-32.3414585302763,5.82169664918694,-0.0558507141174293));
#32456=CARTESIAN_POINT('Ctrl Pts',(-32.2021998861934,5.13581473052646,2.74202082981319));
#32457=CARTESIAN_POINT('Ctrl Pts',(-32.0629412421106,3.19254039164058,4.86856827262033));
#32458=CARTESIAN_POINT('Ctrl Pts',(-31.9236825980277,0.467642045593386,
5.80315277195208));
#32459=CARTESIAN_POINT('Ctrl Pts',(-31.784423953945,-2.37174827385247,5.3169616608454));
#32460=CARTESIAN_POINT('Ctrl Pts',(-31.6451653098621,-4.63046766595764,
3.52902824754106));
#32461=CARTESIAN_POINT('Ctrl Pts',(-31.5059066657793,-5.75551786422157,
0.877089101544608));
#32462=CARTESIAN_POINT('Ctrl Pts',(-31.3666480216964,-5.47145482210148,
-1.98958621505185));
#32463=CARTESIAN_POINT('Ctrl Pts',(-31.2273893776136,-3.84782519086287,
-4.36915466400344));
#32464=CARTESIAN_POINT('Ctrl Pts',(-31.0881307335308,-1.28213933618114,
-5.6790307183567));
#32465=CARTESIAN_POINT('Ctrl Pts',(-30.9488720894479,1.59745042033037,-5.59851974471898));
#32466=CARTESIAN_POINT('Ctrl Pts',(-30.8096134453651,4.08593922098567,-4.14733310210707));
#32467=CARTESIAN_POINT('Ctrl Pts',(-30.6703548012822,5.57407476212171,-1.68076224484598));
#32468=CARTESIAN_POINT('Ctrl Pts',(-30.5310961571994,5.69751945605833,1.19730665464562));
#32469=CARTESIAN_POINT('Ctrl Pts',(-30.3918375131165,4.42605055711307,3.78224108741116));
#32470=CARTESIAN_POINT('Ctrl Pts',(-30.2525788690338,2.07095954287434,5.4411761365719));
#32471=CARTESIAN_POINT('Ctrl Pts',(-30.1133202249508,-0.79116082667304,
5.76795767354096));
#32472=CARTESIAN_POINT('Ctrl Pts',(-29.9740615808681,-3.45958269289924,
4.68258035365267));
#32473=CARTESIAN_POINT('Ctrl Pts',(-29.8348029367852,-5.28100105852438,
2.45077518293425));
#32474=CARTESIAN_POINT('Ctrl Pts',(-29.6955442927024,-5.80948129249884,
-0.381048933246069));
#32475=CARTESIAN_POINT('Ctrl Pts',(-29.5562856486195,-4.91563651556301,
-3.11958151428768));
#32476=CARTESIAN_POINT('Ctrl Pts',(-29.4170270045367,-2.81830516063327,
-5.09435248083305));
#32477=CARTESIAN_POINT('Ctrl Pts',(-29.2777683604539,-0.0309731470350815,
-5.8218821562777));
#32478=CARTESIAN_POINT('Ctrl Pts',(-29.138509716371,2.76394196726982,-5.12405073930642));
#32479=CARTESIAN_POINT('Ctrl Pts',(-28.9992510722882,4.88216606721023,-3.17170705923528));
#32480=CARTESIAN_POINT('Ctrl Pts',(-28.8599924282053,5.80509809971998,-0.442839959860642));
#32481=CARTESIAN_POINT('Ctrl Pts',(-28.7207337841225,5.30677825064084,2.39444686220999));
#32482=CARTESIAN_POINT('Ctrl Pts',(-28.5814751400397,3.50920928564028,4.64550550177244));
#32483=CARTESIAN_POINT('Ctrl Pts',(-28.4422164959568,0.852486829272148,
5.75921326079695));
#32484=CARTESIAN_POINT('Ctrl Pts',(-28.302957851874,-2.01294846696878,5.46290304204184));
#32485=CARTESIAN_POINT('Ctrl Pts',(-28.1636992077911,-4.38555715682404,
3.82911995132712));
#32486=CARTESIAN_POINT('Ctrl Pts',(-28.0244405637083,-5.68445765882755,
1.25786020782067));
#32487=CARTESIAN_POINT('Ctrl Pts',(-27.8851819196254,-5.59164246462076,
-1.62135922153972));
#32488=CARTESIAN_POINT('Ctrl Pts',(-27.7459232755427,-4.12983535374023,
-4.10362414560827));
#32489=CARTESIAN_POINT('Ctrl Pts',(-27.6066646314598,-1.65692797093859,
-5.58120604139851));
#32490=CARTESIAN_POINT('Ctrl Pts',(-27.467405987377,1.22164215104524,-5.69235115152004));
#32491=CARTESIAN_POINT('Ctrl Pts',(-27.3281473432941,3.80111978984003,-4.40984801560195));
#32492=CARTESIAN_POINT('Ctrl Pts',(-27.1888886992113,5.44997600576591,-2.04768960391896));
#32493=CARTESIAN_POINT('Ctrl Pts',(-27.0496300551284,5.76452425311795,0.815801025150685));
#32494=CARTESIAN_POINT('Ctrl Pts',(-26.9103714110456,4.66775424185108,3.4795605347663));
#32495=CARTESIAN_POINT('Ctrl Pts',(-26.7711127669628,2.42818623043581,5.29142540415567));
#32496=CARTESIAN_POINT('Ctrl Pts',(-26.6318541228799,-0.405870313226985,
5.80779996782456));
#32497=CARTESIAN_POINT('Ctrl Pts',(-26.4925954787971,-3.14055834727186,
4.902261156324));
#32498=CARTESIAN_POINT('Ctrl Pts',(-26.3533368347143,-5.10634904597018,
2.79651043233193));
#32499=CARTESIAN_POINT('Ctrl Pts',(-26.2140781906314,-5.82196135578221,
0.00609501438297373));
#32500=CARTESIAN_POINT('Ctrl Pts',(-26.0748195465486,-5.11219318290401,
-2.78581263513747));
#32501=CARTESIAN_POINT('Ctrl Pts',(-25.9355609024658,-3.15081581144937,
-4.89567471343253));
#32502=CARTESIAN_POINT('Ctrl Pts',(-25.7963022583829,-0.418029787868941,
-5.80693742637859));
#32503=CARTESIAN_POINT('Ctrl Pts',(-25.6570436143001,2.41710172796037,-5.29649793864898));
#32504=CARTESIAN_POINT('Ctrl Pts',(-25.5177849702173,4.66045851064236,-3.48932624556705));
#32505=CARTESIAN_POINT('Ctrl Pts',(-25.3785263261344,5.76280349412033,-0.827868990587574));
#32506=CARTESIAN_POINT('Ctrl Pts',(-25.2392676820516,5.45425150935574,2.03627396244039));
#32507=CARTESIAN_POINT('Ctrl Pts',(-25.1000090379688,3.81034479204925,4.40187956935728));
#32508=CARTESIAN_POINT('Ctrl Pts',(-24.9607503938859,1.23355811092897,5.68978080108393));
#32509=CARTESIAN_POINT('Ctrl Pts',(-24.8214917498031,-1.64523841672459,
5.58466308111381));
#32510=CARTESIAN_POINT('Ctrl Pts',(-24.6822331057202,-4.12123413804123,
4.11226219456705));
#32511=CARTESIAN_POINT('Ctrl Pts',(-24.5429744616374,-5.58823540783568,
1.63306344152135));
#32512=CARTESIAN_POINT('Ctrl Pts',(-24.4037158175545,-5.68707890463208,
-1.24595534025541));
#32513=CARTESIAN_POINT('Ctrl Pts',(-24.2644571734717,-4.39356495025238,
-3.81992908380977));
#32514=CARTESIAN_POINT('Ctrl Pts',(-24.1251985293889,-2.02438227414509,
-5.45867635838113));
#32515=CARTESIAN_POINT('Ctrl Pts',(-23.985939885306,0.840426327098998,-5.7609855724642));
#32516=CARTESIAN_POINT('Ctrl Pts',(-23.8466812412232,3.49947483984709,-4.65284289684264));
#32517=CARTESIAN_POINT('Ctrl Pts',(-23.7074225971403,5.30175312834262,-2.40555293924936));
#32518=CARTESIAN_POINT('Ctrl Pts',(-23.5681639530575,5.80601259270488,0.430684282014642));
#32519=CARTESIAN_POINT('Ctrl Pts',(-23.4289053089747,4.88879628178109,3.1614778336508));
#32520=CARTESIAN_POINT('Ctrl Pts',(-23.2896466648918,2.77466463974149,5.11825236915787));
#32521=CARTESIAN_POINT('Ctrl Pts',(-23.150388020809,-0.0187832295640885,
5.82193424625433));
#32522=CARTESIAN_POINT('Ctrl Pts',(-23.0111293767262,-2.80763243405787,
5.10024227783821));
#32523=CARTESIAN_POINT('Ctrl Pts',(-22.8718707326433,-4.90909396461944,
3.12986702975682));
#32524=CARTESIAN_POINT('Ctrl Pts',(-22.7326120885605,-5.80867071834175,
0.393211982651999));
#32525=CARTESIAN_POINT('Ctrl Pts',(-22.5933534444777,-5.28612091258838,
-2.43971245742563));
#32526=CARTESIAN_POINT('Ctrl Pts',(-22.4540948003948,-3.46937949038583,
-4.67532641952538));
#32527=CARTESIAN_POINT('Ctrl Pts',(-22.314836156312,-0.803236035012722,
-5.76628849863402));
#32528=CARTESIAN_POINT('Ctrl Pts',(-22.1755775122291,2.05956227554316,-5.44550038202015));
#32529=CARTESIAN_POINT('Ctrl Pts',(-22.0363188681463,4.41812160355599,-3.79150005586361));
#32530=CARTESIAN_POINT('Ctrl Pts',(-21.8970602240635,5.69500004792524,-1.20923348926227));
#32531=CARTESIAN_POINT('Ctrl Pts',(-21.7578015799806,5.57758172164165,1.66908756985091));
#32532=CARTESIAN_POINT('Ctrl Pts',(-21.6185429358978,4.09461394547347,4.13876887672602));
#32533=CARTESIAN_POINT('Ctrl Pts',(-21.4792842918149,1.60916909236062,5.59516273307697));
#32534=CARTESIAN_POINT('Ctrl Pts',(-21.3400256477321,-1.27024577831713,
5.68170281166567));
#32535=CARTESIAN_POINT('Ctrl Pts',(-21.2007670036493,-3.83866862586252,
4.37720165839326));
#32536=CARTESIAN_POINT('Ctrl Pts',(-21.0615083595664,-5.4672770355491,2.00103797914468));
#32537=CARTESIAN_POINT('Ctrl Pts',(-20.9222497154836,-5.75734169619605,
-0.865036282859993));
#32538=CARTESIAN_POINT('Ctrl Pts',(-20.7829910714007,-4.63784659090838,
-3.51932524450664));
#32539=CARTESIAN_POINT('Ctrl Pts',(-20.6437324273179,-2.38287572265856,
-5.3119840425011));
#32540=CARTESIAN_POINT('Ctrl Pts',(-20.5044737832351,0.455490386506136,
-5.8041191997772));
#32541=CARTESIAN_POINT('Ctrl Pts',(-20.3652151391522,3.18233959143471,-4.8752421378029));
#32542=CARTESIAN_POINT('Ctrl Pts',(-20.2259564950694,5.1300622330414,-2.75276818176615));
#32543=CARTESIAN_POINT('Ctrl Pts',(-20.0866978509866,5.82180082818906,0.0436611305292647));
#32544=CARTESIAN_POINT('Ctrl Pts',(-19.9474392069038,5.08819824233262,2.82940096560128));
#32545=CARTESIAN_POINT('Ctrl Pts',(-19.8081805628209,3.10886109668263,4.92242357573535));
#32546=CARTESIAN_POINT('Ctrl Pts',(-19.6689219187381,0.368386997382966,
5.81029794395959));
#32547=CARTESIAN_POINT('Ctrl Pts',(-19.5296632746552,-2.46227863773393,
5.27564736194346));
#32548=CARTESIAN_POINT('Ctrl Pts',(-19.3904046305724,-4.69010895693356,
3.44936938432428));
#32549=CARTESIAN_POINT('Ctrl Pts',(-19.2511459864896,-5.76966821070186,
0.778588412345258));
#32550=CARTESIAN_POINT('Ctrl Pts',(-19.1118873424067,-5.43664981983068,
-2.08281298103237));
#32551=CARTESIAN_POINT('Ctrl Pts',(-18.9726286983239,-3.77258608687527,
-4.43428296284045));
#32552=CARTESIAN_POINT('Ctrl Pts',(-18.8333700542411,-1.18488678698841,
-5.70011530404799));
#32553=CARTESIAN_POINT('Ctrl Pts',(-18.6941114101582,1.69290624543302,-5.57039851550999));
#32554=CARTESIAN_POINT('Ctrl Pts',(-18.5548527660754,4.15622804147844,-4.07689092871645));
#32555=CARTESIAN_POINT('Ctrl Pts',(-18.4155941219925,5.60198789062944,-1.58524535976706));
#32556=CARTESIAN_POINT('Ctrl Pts',(-18.2763354779097,5.67622297078826,1.29451302168715));
#32557=CARTESIAN_POINT('Ctrl Pts',(-18.1370768338268,4.36075843881821,3.85733807381434));
#32558=CARTESIAN_POINT('Ctrl Pts',(-17.997818189744,1.97765714518448,5.47577788022147));
#32559=CARTESIAN_POINT('Ctrl Pts',(-17.8585595456612,-0.889630443055851,
5.75359269085066));
#32560=CARTESIAN_POINT('Ctrl Pts',(-17.7193009015783,-3.53911138627618,
4.62276559788101));
#32561=CARTESIAN_POINT('Ctrl Pts',(-17.5800422574955,-5.32211795981442,
2.36015499474989));
#32562=CARTESIAN_POINT('Ctrl Pts',(-17.4407836134127,-5.80211982361497,
-0.480288173741599));
#32563=CARTESIAN_POINT('Ctrl Pts',(-17.3015249693298,-4.86159897188818,
-3.20314323968782));
#32564=CARTESIAN_POINT('Ctrl Pts',(-17.162266325247,-2.73082145823515,-5.14177842197275));
#32565=CARTESIAN_POINT('Ctrl Pts',(-17.0230076811641,0.0685382342422849,
-5.82156110402261));
#32566=CARTESIAN_POINT('Ctrl Pts',(-16.8837490370813,2.85111783227435,-5.07606129631125));
#32567=CARTESIAN_POINT('Ctrl Pts',(-16.7444903929985,4.93566330338145,-3.08779839579521));
#32568=CARTESIAN_POINT('Ctrl Pts',(-16.6052317489156,5.81181907351895,-0.343555285366334));
#32569=CARTESIAN_POINT('Ctrl Pts',(-16.4659731048328,5.26507747796142,2.48479985682658));
#32570=CARTESIAN_POINT('Ctrl Pts',(-16.32671446075,3.42929629276711,4.7048058529376));
#32571=CARTESIAN_POINT('Ctrl Pts',(-16.1874558166671,0.753926572650982,
5.77294256861028));
#32572=CARTESIAN_POINT('Ctrl Pts',(-16.0481971725843,-2.10602565435016,
5.42769998439863));
#32573=CARTESIAN_POINT('Ctrl Pts',(-15.9089385285014,-4.45036335210432,
3.7536032304532));
#32574=CARTESIAN_POINT('Ctrl Pts',(-15.7696798844186,-5.70512647604768,
1.16051844867799));
#32575=CARTESIAN_POINT('Ctrl Pts',(-15.6304212403358,-5.56311359388409,
-1.716694008542));
#32576=CARTESIAN_POINT('Ctrl Pts',(-15.4911625962529,-4.05909346791839,
-4.17361131349388));
#32577=CARTESIAN_POINT('Ctrl Pts',(-15.3519039521701,-1.56129268058847,
-5.60871075586562));
#32578=CARTESIAN_POINT('Ctrl Pts',(-15.2126453080873,1.31875662724521,-5.67063948206185));
#32579=CARTESIAN_POINT('Ctrl Pts',(-15.0733866640044,3.87593708676088,-4.34423559178062));
#32580=CARTESIAN_POINT('Ctrl Pts',(-14.9341280199216,5.48417873717277,-1.95424019919872));
#32581=CARTESIAN_POINT('Ctrl Pts',(-14.7948693758387,5.7497386248849,0.914208358597051));
#32582=CARTESIAN_POINT('Ctrl Pts',(-14.6556107317559,4.60760019313947,3.55883290386089));
#32583=CARTESIAN_POINT('Ctrl Pts',(-14.5163520876731,2.33739117040358,5.33215469523732));
#32584=CARTESIAN_POINT('Ctrl Pts',(-14.3770934435902,-0.505077190913626,
5.80001450072677));
#32585=CARTESIAN_POINT('Ctrl Pts',(-14.2378347995074,-3.22388839853548,
4.8478670331611));
#32586=CARTESIAN_POINT('Ctrl Pts',(-14.0985761554245,-5.15340072201409,
2.70882486989593));
#32587=CARTESIAN_POINT('Ctrl Pts',(-13.9593175113417,-5.82121507813234,
-0.0934140864467144));
#32588=CARTESIAN_POINT('Ctrl Pts',(-13.8200588672589,-5.06383166139498,
-2.87278263752683));
#32589=CARTESIAN_POINT('Ctrl Pts',(-13.680800223176,-3.06667931169952,-4.94881290580035));
#32590=CARTESIAN_POINT('Ctrl Pts',(-13.5415415790932,-0.318717300028964,
-5.81323407924405));
#32591=CARTESIAN_POINT('Ctrl Pts',(-13.4022829350104,2.50727570346634,-5.25441145364819));
#32592=CARTESIAN_POINT('Ctrl Pts',(-13.2630242909275,4.71941683917222,-3.40916058224889));
#32593=CARTESIAN_POINT('Ctrl Pts',(-13.1237656468447,5.77611151256949,-0.729250966255149));
#32594=CARTESIAN_POINT('Ctrl Pts',(-12.9845070027619,5.41865103914805,2.12919987163296));
#32595=CARTESIAN_POINT('Ctrl Pts',(-12.845248358679,3.73455183322449,4.46636247771959));
#32596=CARTESIAN_POINT('Ctrl Pts',(-12.7059897145962,1.1361289192972,5.71003347242015));
#32597=CARTESIAN_POINT('Ctrl Pts',(-12.5667310705133,-1.74045042481285,
5.55572708978679));
#32598=CARTESIAN_POINT('Ctrl Pts',(-12.4274724264305,-4.1909183753537,4.04122188806115));
#32599=CARTESIAN_POINT('Ctrl Pts',(-12.2882137823477,-5.61533120602602,
1.5373114922007));
#32600=CARTESIAN_POINT('Ctrl Pts',(-12.1489551382648,-5.6649524474409,-1.34297615230335));
#32601=CARTESIAN_POINT('Ctrl Pts',(-12.009696494182,-4.32763341898751,-3.89446532508437));
#32602=CARTESIAN_POINT('Ctrl Pts',(-11.8704378500991,-1.93078756878074,
-5.49247945300331));
#32603=CARTESIAN_POINT('Ctrl Pts',(-11.7311792060163,0.938769580690719,
-5.745779568674));
#32604=CARTESIAN_POINT('Ctrl Pts',(-11.5919205619335,3.57848943714567,-4.59235065360418));
#32605=CARTESIAN_POINT('Ctrl Pts',(-11.4526619178506,5.34209406549889,-2.31458466528736));
#32606=CARTESIAN_POINT('Ctrl Pts',(-11.3134032737678,5.79780326955581,0.52985698537453));
#32607=CARTESIAN_POINT('Ctrl Pts',(-11.174144629685,4.83404657236697,3.244574689171));
#32608=CARTESIAN_POINT('Ctrl Pts',(-11.0348859856021,2.68677881840614,5.16492892094228));
#32609=CARTESIAN_POINT('Ctrl Pts',(-10.8956273415193,-0.118288232909747,
5.82076275683669));
#32610=CARTESIAN_POINT('Ctrl Pts',(-10.7563686974365,-2.8943949857596,5.05150956089681));
#32611=CARTESIAN_POINT('Ctrl Pts',(-10.6171100533536,-4.96187214288032,
3.04550423002994));
#32612=CARTESIAN_POINT('Ctrl Pts',(-10.4778514092708,-5.81454293529678,
0.2938734949127));
#32613=CARTESIAN_POINT('Ctrl Pts',(-10.3385927651879,-5.24364948376559,
-2.52970576724383));
#32614=CARTESIAN_POINT('Ctrl Pts',(-10.1993341211051,-3.38896262044802,
-4.73394164884063));
#32615=CARTESIAN_POINT('Ctrl Pts',(-10.0600754770223,-0.704562043734518,
-5.77917498471456));
#32616=CARTESIAN_POINT('Ctrl Pts',(-9.92081683293943,2.15233520971946,-5.4095031493127));
#32617=CARTESIAN_POINT('Ctrl Pts',(-9.78155818885659,4.48228004754217,-3.71543224306774));
#32618=CARTESIAN_POINT('Ctrl Pts',(-9.64229954477375,5.71483620356373,-1.11171864419876));
#32619=CARTESIAN_POINT('Ctrl Pts',(-9.50304090069091,5.54823913809556,1.76417506045364));
#32620=CARTESIAN_POINT('Ctrl Pts',(-9.36378225660808,4.02327651547963,4.20814891103108));
#32621=CARTESIAN_POINT('Ctrl Pts',(-9.22452361252525,1.51330223250026,5.62184912022118));
#32622=CARTESIAN_POINT('Ctrl Pts',(-9.08526496844239,-1.36717115461266,
5.65916197077067));
#32623=CARTESIAN_POINT('Ctrl Pts',(-8.94600632435957,-3.91292245045877,
4.31095222359489));
#32624=CARTESIAN_POINT('Ctrl Pts',(-8.80674768027673,-5.50067987614199,
1.90729968217594));
#32625=CARTESIAN_POINT('Ctrl Pts',(-8.66748903619388,-5.74171559451039,
-0.96331366084895));
#32626=CARTESIAN_POINT('Ctrl Pts',(-8.52823039211106,-4.57701725773164,
-3.59808062720235));
#32627=CARTESIAN_POINT('Ctrl Pts',(-8.38897174802821,-2.29173589584776,
-5.35193588910637));
#32628=CARTESIAN_POINT('Ctrl Pts',(-8.24971310394538,0.554627104645345,
-5.79548617047911));
#32629=CARTESIAN_POINT('Ctrl Pts',(-8.11045445986253,3.26520173386261,-4.82013784186744));
#32630=CARTESIAN_POINT('Ctrl Pts',(-7.9711958157797,5.17636280825239,-2.6646837063268));
#32631=CARTESIAN_POINT('Ctrl Pts',(-7.83193717169687,5.82020414839504,0.143160219429282));
#32632=CARTESIAN_POINT('Ctrl Pts',(-7.69267852761401,5.0390952198184,2.91595448233083));
#32633=CARTESIAN_POINT('Ctrl Pts',(-7.5534198835312,3.02427353744386,4.97484077615946));
#32634=CARTESIAN_POINT('Ctrl Pts',(-7.41416123944835,0.269024323665677,
5.81574561777749));
#32635=CARTESIAN_POINT('Ctrl Pts',(-7.27490259536551,-2.55208963858617,
5.23279176482717));
#32636=CARTESIAN_POINT('Ctrl Pts',(-7.13564395128268,-4.74838001671997,
3.36870277617907));
#32637=CARTESIAN_POINT('Ctrl Pts',(-6.99638530719984,-5.78213292910652,
0.679860255908561));
#32638=CARTESIAN_POINT('Ctrl Pts',(-6.85712666311699,-5.400256481933,-2.17543124615844));
#32639=CARTESIAN_POINT('Ctrl Pts',(-6.71786801903417,-3.69624480910674,
-4.49811577091712));
#32640=CARTESIAN_POINT('Ctrl Pts',(-6.57860937495133,-1.08728806911454,
-5.71953458178049));
#32641=CARTESIAN_POINT('Ctrl Pts',(-6.43935073086849,1.78786748225226,-5.5406498755405));
#32642=CARTESIAN_POINT('Ctrl Pts',(-6.30009208678565,4.22530260589625,-4.00525767785651));
#32643=CARTESIAN_POINT('Ctrl Pts',(-6.16083344270281,5.62826437943398,-1.48926533989636));
#32644=CARTESIAN_POINT('Ctrl Pts',(-6.02157479861997,5.65326815778531,1.39134119237251));
#32645=CARTESIAN_POINT('Ctrl Pts',(-5.88231615453714,4.29419231020122,3.93130812585718));
#32646=CARTESIAN_POINT('Ctrl Pts',(-5.74305751045431,1.88377696827288,5.50877985684914));
#32647=CARTESIAN_POINT('Ctrl Pts',(-5.60379886637146,-0.987840150896906,
5.73754677660216));
#32648=CARTESIAN_POINT('Ctrl Pts',(-5.46454022228862,-3.6176061162956,4.56160028550974));
#32649=CARTESIAN_POINT('Ctrl Pts',(-5.32528157820579,-5.36167998634783,
2.26884527930375));
#32650=CARTESIAN_POINT('Ctrl Pts',(-5.18602293412295,-5.793063245807,-0.579387096423341));
#32651=CARTESIAN_POINT('Ctrl Pts',(-5.04676429004011,-4.80614109563603,
-3.28576915596036));
#32652=CARTESIAN_POINT('Ctrl Pts',(-4.90750564595728,-2.64253993711476,
-5.18770217516153));
#32653=CARTESIAN_POINT('Ctrl Pts',(-4.76824700187443,0.16802959184276,-5.81953926300762));
#32654=CARTESIAN_POINT('Ctrl Pts',(-4.6289883577916,2.93746073356423,-5.02658886484561));
#32655=CARTESIAN_POINT('Ctrl Pts',(-4.48972971370876,4.98771856883065,-3.00298762161356));
#32656=CARTESIAN_POINT('Ctrl Pts',(-4.35047106962593,5.81684210472518,-0.244170240033472));
#32657=CARTESIAN_POINT('Ctrl Pts',(-4.21121242554308,5.2218384950949,2.57442690876366));
#32658=CARTESIAN_POINT('Ctrl Pts',(-4.07195378146025,3.34838141938695,4.76273167916573));
#32659=CARTESIAN_POINT('Ctrl Pts',(-3.93269513737742,0.655146053832615,
5.78498529173258));
#32660=CARTESIAN_POINT('Ctrl Pts',(-3.79343649329457,-2.1984875592163,5.39091120585453));
#32661=CARTESIAN_POINT('Ctrl Pts',(-3.65417784921174,-4.51386935868354,
3.67698988170163));
#32662=CARTESIAN_POINT('Ctrl Pts',(-3.5149192051289,-5.72412852127934,1.06283764015143));
#32663=CARTESIAN_POINT('Ctrl Pts',(-3.37566056104605,-5.53295944069909,
-1.81152725759464));
#32664=CARTESIAN_POINT('Ctrl Pts',(-3.23640191696322,-3.98716570422026,
-4.24237914670461));
#32665=CARTESIAN_POINT('Ctrl Pts',(-3.09714327288039,-1.46520125329375,
-5.6345768665572));
#32666=CARTESIAN_POINT('Ctrl Pts',(-2.95788462879754,1.41548582422035,-5.64727111603672));
#32667=CARTESIAN_POINT('Ctrl Pts',(-2.81862598471471,3.94962201559119,-4.27735398497753));
#32668=CARTESIAN_POINT('Ctrl Pts',(-2.67936734063188,5.51677924715227,-1.8602198563335));
#32669=CARTESIAN_POINT('Ctrl Pts',(-2.54010869654903,5.73327319120209,1.01234860246717));
#32670=CARTESIAN_POINT('Ctrl Pts',(-2.4008500524662,4.54610001819894,3.63706554889101));
#32671=CARTESIAN_POINT('Ctrl Pts',(-2.26159140838336,2.24591323413269,5.37132617734322));
#32672=CARTESIAN_POINT('Ctrl Pts',(-2.12233276430053,-0.604136509556456,
5.79053454359149));
#32673=CARTESIAN_POINT('Ctrl Pts',(-1.98307412021767,-3.30627657802072,
4.79205658182243));
#32674=CARTESIAN_POINT('Ctrl Pts',(-1.84381547613485,-5.19894681828512,
2.62034792960979));
#32675=CARTESIAN_POINT('Ctrl Pts',(-1.70455683205201,-5.81876810565199,
-0.192895924308944));
#32676=CARTESIAN_POINT('Ctrl Pts',(-1.56529818796917,-5.01399073831737,
-2.9589132916041));
#32677=CARTESIAN_POINT('Ctrl Pts',(-1.42603954388634,-2.98164684396445,
-5.00050539332495));
#32678=CARTESIAN_POINT('Ctrl Pts',(-1.2867808998035,-0.219311751017547,
-5.81783216627008));
#32679=CARTESIAN_POINT('Ctrl Pts',(-1.14752225572065,2.59671727360405,-5.21079028391074));
#32680=CARTESIAN_POINT('Ctrl Pts',(-1.00826361163782,4.77699617182404,-3.32799812267906));
#32681=CARTESIAN_POINT('Ctrl Pts',(-0.869004967554989,5.78773241510616,
-0.630421446287272));
#32682=CARTESIAN_POINT('Ctrl Pts',(-0.729746323472141,5.381466722009,2.22150676598878));
#32683=CARTESIAN_POINT('Ctrl Pts',(-0.5904876793893,3.65766931387145,4.52953459695107));
#32684=CARTESIAN_POINT('Ctrl Pts',(-0.451229035306472,1.03836487504737,
5.72862949825498));
#32685=CARTESIAN_POINT('Ctrl Pts',(-0.311970391223629,-1.83514824151881,
5.52514542236776));
#32686=CARTESIAN_POINT('Ctrl Pts',(-0.172711747140795,-4.25938936625894,
3.96904493801873));
#32687=CARTESIAN_POINT('Ctrl Pts',(-0.0334531030579666,-5.64076471879598,
1.44102431516129));
#32688=CARTESIAN_POINT('Ctrl Pts',(0.105805541024883,-5.64121346572028,
-1.43943410988536));
#32689=CARTESIAN_POINT('Ctrl Pts',(0.245064185107723,-4.26035369318523,
-3.96822316047526));
#32690=CARTESIAN_POINT('Ctrl Pts',(0.337903281162944,-2.64465155276186,
-5.00520070296182));
#32691=CARTESIAN_POINT('Ctrl Pts',(0.384322829190555,-1.76153289128266,
-5.29878544698756));
#32692=CARTESIAN_POINT('Ctrl Pts',(-59.58325,-2.58391981634379,5.32271443393368));
#32693=CARTESIAN_POINT('Ctrl Pts',(-59.5368304519724,-3.47102658701026,
4.89206710306723));
#32694=CARTESIAN_POINT('Ctrl Pts',(-59.4439913559172,-5.02484286868922,
3.57907156976542));
#32695=CARTESIAN_POINT('Ctrl Pts',(-59.3047327118343,-6.125475880775,0.731390377776202));
#32696=CARTESIAN_POINT('Ctrl Pts',(-59.1654740677516,-5.72633323264516,
-2.29454852325651));
#32697=CARTESIAN_POINT('Ctrl Pts',(-59.0262154236686,-3.925268426147,-4.75911398603417));
#32698=CARTESIAN_POINT('Ctrl Pts',(-58.8869567795858,-1.16316343878524,
-6.05831220422429));
#32699=CARTESIAN_POINT('Ctrl Pts',(-58.747698135503,1.88370464411569,-5.87436787906887));
#32700=CARTESIAN_POINT('Ctrl Pts',(-58.6084394914201,4.46939488601017,-4.25215953310488));
#32701=CARTESIAN_POINT('Ctrl Pts',(-58.4691808473373,5.96084790378021,-1.58892964266834));
#32702=CARTESIAN_POINT('Ctrl Pts',(-58.3299222032545,5.99291872863358,1.46332898982328));
#32703=CARTESIAN_POINT('Ctrl Pts',(-58.1906635591716,4.55775304079097,4.15731624602566));
#32704=CARTESIAN_POINT('Ctrl Pts',(-58.0514049150888,2.00672118223107,5.83347878871376));
#32705=CARTESIAN_POINT('Ctrl Pts',(-57.912146271006,-1.03561288821634,6.08143918145384));
#32706=CARTESIAN_POINT('Ctrl Pts',(-57.7728876269232,-3.82439957717761,
4.84049255622217));
#32707=CARTESIAN_POINT('Ctrl Pts',(-57.6336289828403,-5.6768653521605,2.41445622274904));
#32708=CARTESIAN_POINT('Ctrl Pts',(-57.4943703387574,-6.13947421220047,
-0.602706896951242));
#32709=CARTESIAN_POINT('Ctrl Pts',(-57.3551116946747,-5.09896649475701,
-3.47231048449872));
#32710=CARTESIAN_POINT('Ctrl Pts',(-57.2158530505918,-2.81008783754839,
-5.49179438240193));
#32711=CARTESIAN_POINT('Ctrl Pts',(-57.0765944065089,0.166779641673839,
-6.16673202670761));
#32712=CARTESIAN_POINT('Ctrl Pts',(-56.9373357624261,3.10281475879802,-5.33187957842086));
#32713=CARTESIAN_POINT('Ctrl Pts',(-56.7980771183432,5.2791932354107,-3.19163250955323));
#32714=CARTESIAN_POINT('Ctrl Pts',(-56.6588184742605,6.16307618704186,-0.269983704102151));
#32715=CARTESIAN_POINT('Ctrl Pts',(-56.5195598301775,5.5380641159968,2.71776473088446));
#32716=CARTESIAN_POINT('Ctrl Pts',(-56.3803011860948,3.5571776205769,5.04012764367346));
#32717=CARTESIAN_POINT('Ctrl Pts',(-56.2410425420118,0.705393631270256,
6.12852503554376));
#32718=CARTESIAN_POINT('Ctrl Pts',(-56.1017838979292,-2.31909063084241,
5.71648650253054));
#32719=CARTESIAN_POINT('Ctrl Pts',(-55.9625252538461,-4.77579604306655,
3.90489070809336));
#32720=CARTESIAN_POINT('Ctrl Pts',(-55.8232666097635,-6.06325177238225,
1.13726744082824));
#32721=CARTESIAN_POINT('Ctrl Pts',(-55.6840079656805,-5.86625231386363,
-1.90879099887135));
#32722=CARTESIAN_POINT('Ctrl Pts',(-55.5447493215978,-4.23302869586511,
-4.48752352051908));
#32723=CARTESIAN_POINT('Ctrl Pts',(-55.4054906775148,-1.56344016284461,
-5.967583610179));
#32724=CARTESIAN_POINT('Ctrl Pts',(-55.2662320334321,1.48892265495596,-5.98661077862981));
#32725=CARTESIAN_POINT('Ctrl Pts',(-55.1269733893491,4.17675517739415,-4.539946637943));
#32726=CARTESIAN_POINT('Ctrl Pts',(-54.9877147452664,5.84200013062435,-1.98177540630629));
#32727=CARTESIAN_POINT('Ctrl Pts',(-54.8484561011835,6.07695854342666,1.06159038650946));
#32728=CARTESIAN_POINT('Ctrl Pts',(-54.7091974571007,4.82410596392218,3.84504888604902));
#32729=CARTESIAN_POINT('Ctrl Pts',(-54.5699388130179,2.39017606919722,5.68713087993344));
#32730=CARTESIAN_POINT('Ctrl Pts',(-54.430680168935,-0.628936397350093,
6.13684269762101));
#32731=CARTESIAN_POINT('Ctrl Pts',(-54.2914215248522,-3.49406748015876,
5.08408219164018));
#32732=CARTESIAN_POINT('Ctrl Pts',(-54.1521628807693,-5.50375221300585,
2.78659485126364));
#32733=CARTESIAN_POINT('Ctrl Pts',(-54.0129042366865,-6.16596304374769,
-0.193129568926519));
#32734=CARTESIAN_POINT('Ctrl Pts',(-53.8736455926037,-5.31857206807786,
-3.12557041896641));
#32735=CARTESIAN_POINT('Ctrl Pts',(-53.7343869485208,-3.1690445170612,-5.29278340158939));
#32736=CARTESIAN_POINT('Ctrl Pts',(-53.595128304438,-0.243645412223681,
-6.16417360238647));
#32737=CARTESIAN_POINT('Ctrl Pts',(-53.4558696603552,2.74140496716854,-5.52640010252963));
#32738=CARTESIAN_POINT('Ctrl Pts',(-53.3166110162723,5.05528202599734,-3.53560785790563));
#32739=CARTESIAN_POINT('Ctrl Pts',(-53.1773523721895,6.13148334395316,-0.679199006242515));
#32740=CARTESIAN_POINT('Ctrl Pts',(-53.0380937281066,5.70652445930279,2.34349693463311));
#32741=CARTESIAN_POINT('Ctrl Pts',(-52.8988350840238,3.88444730278233,4.79243867349005));
#32742=CARTESIAN_POINT('Ctrl Pts',(-52.759576439941,1.11134779604893,6.06805614373112));
#32743=CARTESIAN_POINT('Ctrl Pts',(-52.6203177958581,-1.93384102237248,
5.85804218040851));
#32744=CARTESIAN_POINT('Ctrl Pts',(-52.4810591517753,-4.50557096989672,
4.21381413003465));
#32745=CARTESIAN_POINT('Ctrl Pts',(-52.3418005076924,-5.97420996036946,
1.53792543274314));
#32746=CARTESIAN_POINT('Ctrl Pts',(-52.2025418636096,-5.98019371206306,
-1.51449082316711));
#32747=CARTESIAN_POINT('Ctrl Pts',(-52.0632832195268,-4.52205723365308,
-4.19611697439688));
#32748=CARTESIAN_POINT('Ctrl Pts',(-51.9240245754439,-1.95679349544846,
-5.85041524196586));
#32749=CARTESIAN_POINT('Ctrl Pts',(-51.7847659313611,1.08754852696658,-6.0723667123082));
#32750=CARTESIAN_POINT('Ctrl Pts',(-51.6455072872782,3.86562797057267,-4.80763140022008));
#32751=CARTESIAN_POINT('Ctrl Pts',(-51.5062486431954,5.69729256772438,-2.36585221115108));
#32752=CARTESIAN_POINT('Ctrl Pts',(-51.3669899991126,6.13409912066294,0.655154382674766));
#32753=CARTESIAN_POINT('Ctrl Pts',(-51.2277313550298,5.06910505501842,3.51576068987105));
#32754=CARTESIAN_POINT('Ctrl Pts',(-51.0884727109469,2.76305098079898,5.51560953701054));
#32755=CARTESIAN_POINT('Ctrl Pts',(-50.9492140668641,-0.21947596914604,
6.16508147441892));
#32756=CARTESIAN_POINT('Ctrl Pts',(-50.8099554227812,-3.14826900645875,
5.30516743847233));
#32757=CARTESIAN_POINT('Ctrl Pts',(-50.6706967786984,-5.30627692139886,
3.14639865889332));
#32758=CARTESIAN_POINT('Ctrl Pts',(-50.5314381346156,-6.16515845996755,
0.217302670822068));
#32759=CARTESIAN_POINT('Ctrl Pts',(-50.3921794905327,-5.51463517694584,
-2.76499514510376));
#32760=CARTESIAN_POINT('Ctrl Pts',(-50.2529208464499,-3.51397353504114,
-5.07034409900219));
#32761=CARTESIAN_POINT('Ctrl Pts',(-50.113662202367,-0.652991979029951,
-6.13432969138262));
#32762=CARTESIAN_POINT('Ctrl Pts',(-49.9744035582842,2.36786044615801,-5.6964582149592));
#32763=CARTESIAN_POINT('Ctrl Pts',(-49.8351449142013,4.80899379397081,-3.86393296743177));
#32764=CARTESIAN_POINT('Ctrl Pts',(-49.6958862701186,6.07274971235482,-1.08540785806552));
#32765=CARTESIAN_POINT('Ctrl Pts',(-49.5566276260357,5.84972507908559,1.95885573393575));
#32766=CARTESIAN_POINT('Ctrl Pts',(-49.4173689819528,4.19452261994479,4.52353614753185));
#32767=CARTESIAN_POINT('Ctrl Pts',(-49.2781103378701,1.51238262011864,5.98072722146889));
#32768=CARTESIAN_POINT('Ctrl Pts',(-49.1388516937871,-1.54003133677118,
5.97366744713988));
#32769=CARTESIAN_POINT('Ctrl Pts',(-48.9995930497044,-4.2154021502906,4.50408525658442));
#32770=CARTESIAN_POINT('Ctrl Pts',(-48.8603344056215,-5.85872352470692,
1.93177585353516));
#32771=CARTESIAN_POINT('Ctrl Pts',(-48.7210757615387,-6.06766399975473,
-1.11348680878414));
#32772=CARTESIAN_POINT('Ctrl Pts',(-48.5818171174559,-4.79106904915372,
-3.88613646871764));
#32773=CARTESIAN_POINT('Ctrl Pts',(-48.4425584733729,-2.34148515263626,
-5.70735022293531));
#32774=CARTESIAN_POINT('Ctrl Pts',(-48.3032998292902,0.681360404878315,
-6.13124353503593));
#32775=CARTESIAN_POINT('Ctrl Pts',(-48.1640411852073,3.5373897017822,-5.05403535652265));
#32776=CARTESIAN_POINT('Ctrl Pts',(-48.0247825411245,5.52736614596797,-2.73945665701488));
#32777=CARTESIAN_POINT('Ctrl Pts',(-47.8855238970416,6.1640873306833,0.245818361733667));
#32778=CARTESIAN_POINT('Ctrl Pts',(-47.7462652529589,5.29166593649294,3.17091010654926));
#32779=CARTESIAN_POINT('Ctrl Pts',(-47.6070066088759,3.12369534747615,5.31967354857529));
#32780=CARTESIAN_POINT('Ctrl Pts',(-47.4677479647933,0.190955961472976,
6.16603074173603));
#32781=CARTESIAN_POINT('Ctrl Pts',(-47.3284893207102,-2.78853483421908,
5.50276955410661));
#32782=CARTESIAN_POINT('Ctrl Pts',(-47.1892306766276,-5.08531358750806,
3.49227504700901));
#32783=CARTESIAN_POINT('Ctrl Pts',(-47.0499720325445,-6.13706402593289,
0.626773028181855));
#32784=CARTESIAN_POINT('Ctrl Pts',(-46.9107133884618,-5.68628795327095,
-2.3921807205438));
#32785=CARTESIAN_POINT('Ctrl Pts',(-46.7714547443789,-3.84334807665325,
-4.82546110220999));
#32786=CARTESIAN_POINT('Ctrl Pts',(-46.6321961002961,-1.05944810053127,
-6.07733239254992));
#32787=CARTESIAN_POINT('Ctrl Pts',(-46.4929374562133,1.98383467678721,-5.84130116176459));
#32788=CARTESIAN_POINT('Ctrl Pts',(-46.3536788121304,4.54141872538288,-4.1751545178589));
#32789=CARTESIAN_POINT('Ctrl Pts',(-46.2144201680476,5.98713527447069,-1.48681219138281));
#32790=CARTESIAN_POINT('Ctrl Pts',(-46.0751615239648,5.96703210303059,1.56554372939827));
#32791=CARTESIAN_POINT('Ctrl Pts',(-45.9359028798819,4.48603103490502,4.23461035292798));
#32792=CARTESIAN_POINT('Ctrl Pts',(-45.7966442357991,1.90672293738878,5.86692482713825));
#32793=CARTESIAN_POINT('Ctrl Pts',(-45.6573855917162,-1.13940475832912,
6.06285049163781));
#32794=CARTESIAN_POINT('Ctrl Pts',(-45.5181269476334,-3.90657400599862,
4.77441921315165));
#32795=CARTESIAN_POINT('Ctrl Pts',(-45.3788683035505,-5.71730366191351,
2.31707533859527));
#32796=CARTESIAN_POINT('Ctrl Pts',(-45.2396096594678,-6.12827599288294,
-0.707553985438834));
#32797=CARTESIAN_POINT('Ctrl Pts',(-45.1003510153848,-5.03887337132555,
-3.55895412094651));
#32798=CARTESIAN_POINT('Ctrl Pts',(-44.9610923713022,-2.71581231074366,
-5.53902182520244));
#32799=CARTESIAN_POINT('Ctrl Pts',(-44.8218337272191,0.272156265677259,
-6.16298063069392));
#32800=CARTESIAN_POINT('Ctrl Pts',(-44.6825750831364,3.19349330581138,-5.27806780867713));
#32801=CARTESIAN_POINT('Ctrl Pts',(-44.5433164390535,5.33297303849622,-3.10093499737228));
#32802=CARTESIAN_POINT('Ctrl Pts',(-44.4040577949708,6.16679043176404,-0.16460576526746));
#32803=CARTESIAN_POINT('Ctrl Pts',(-44.2647991508878,5.49080345067826,2.81202360467965));
#32804=CARTESIAN_POINT('Ctrl Pts',(-44.1255405068051,3.4705127900237,5.10019021817205));
#32805=CARTESIAN_POINT('Ctrl Pts',(-43.9862818627222,0.60054263245633,6.13968629767501));
#32806=CARTESIAN_POINT('Ctrl Pts',(-43.8470232186394,-2.4164573137022,5.67601385994704));
#32807=CARTESIAN_POINT('Ctrl Pts',(-43.7077645745565,-4.84184029751447,
3.82269300632694));
#32808=CARTESIAN_POINT('Ctrl Pts',(-43.5685059304737,-6.08180410063669,
1.03346899747141));
#32809=CARTESIAN_POINT('Ctrl Pts',(-43.4292472863909,-5.83277058226627,
-2.00877739481134));
#32810=CARTESIAN_POINT('Ctrl Pts',(-43.289988642308,-4.15571017743855,-4.55921837691391));
#32811=CARTESIAN_POINT('Ctrl Pts',(-43.1507299982251,-1.46121461345175,
-5.99343400236382));
#32812=CARTESIAN_POINT('Ctrl Pts',(-43.0114713541424,1.59102753519202,-5.9602878008966));
#32813=CARTESIAN_POINT('Ctrl Pts',(-42.8722127100595,4.25374123156719,-4.46789489828499));
#32814=CARTESIAN_POINT('Ctrl Pts',(-42.7329540659767,5.87501899950408,-1.88163520447562));
#32815=CARTESIAN_POINT('Ctrl Pts',(-42.5936954218938,6.05792627585209,1.16530190233972));
#32816=CARTESIAN_POINT('Ctrl Pts',(-42.454436777811,4.75768219623993,3.92694020922617));
#32817=CARTESIAN_POINT('Ctrl Pts',(-42.3151781337282,2.29262321475141,5.72715270290909));
#32818=CARTESIAN_POINT('Ctrl Pts',(-42.1759194896453,-0.733734646061337,
6.12519654839133));
#32819=CARTESIAN_POINT('Ctrl Pts',(-42.0366608455625,-3.58045355359749,
5.0236193762851));
#32820=CARTESIAN_POINT('Ctrl Pts',(-41.8974022014796,-5.5505763618812,2.69211837373126));
#32821=CARTESIAN_POINT('Ctrl Pts',(-41.7581435573968,-6.1617613946591,-0.298489200046597));
#32822=CARTESIAN_POINT('Ctrl Pts',(-41.6188849133139,-5.26437330332677,
-3.21601819187584));
#32823=CARTESIAN_POINT('Ctrl Pts',(-41.4796262692311,-3.07811802418573,
-5.34617514831293));
#32824=CARTESIAN_POINT('Ctrl Pts',(-41.3403676251482,-0.13825256336012,
-6.16743751617966));
#32825=CARTESIAN_POINT('Ctrl Pts',(-41.2011089810655,2.83546102758053,-5.47873708516185));
#32826=CARTESIAN_POINT('Ctrl Pts',(-41.0618503369825,5.11497371934684,-3.44868716146404));
#32827=CARTESIAN_POINT('Ctrl Pts',(-40.9225916928999,6.14219645872631,-0.57430127082044));
#32828=CARTESIAN_POINT('Ctrl Pts',(-40.7833330488169,5.66563612259242,2.44068978234263));
#32829=CARTESIAN_POINT('Ctrl Pts',(-40.6440744047341,3.8019681336144,4.85813108080016));
#32830=CARTESIAN_POINT('Ctrl Pts',(-40.5048157606512,1.0074710232644,6.08616475496173));
#32831=CARTESIAN_POINT('Ctrl Pts',(-40.3655571165684,-2.03368343255402,
5.82413349635901));
#32832=CARTESIAN_POINT('Ctrl Pts',(-40.2262984724856,-4.57693477710325,
4.13618995373747));
#32833=CARTESIAN_POINT('Ctrl Pts',(-40.0870398284027,-5.99962329013349,
1.4355903537373));
#32834=CARTESIAN_POINT('Ctrl Pts',(-39.9477811843199,-5.95343466388885,
-1.61648228881805));
#32835=CARTESIAN_POINT('Ctrl Pts',(-39.8085225402371,-4.44967717789028,
-4.27279443687832));
#32836=CARTESIAN_POINT('Ctrl Pts',(-39.6692638961542,-1.85651311289782,
-5.88300589400472));
#32837=CARTESIAN_POINT('Ctrl Pts',(-39.5300052520714,1.19117776793395,-6.05289144231381));
#32838=CARTESIAN_POINT('Ctrl Pts',(-39.3907466079885,3.94723470651334,-4.74085830403655));
#32839=CARTESIAN_POINT('Ctrl Pts',(-39.2514879639057,5.73689716607855,-2.26812922760052));
#32840=CARTESIAN_POINT('Ctrl Pts',(-39.1122293198229,6.12200525779175,0.75990190868693));
#32841=CARTESIAN_POINT('Ctrl Pts',(-38.97297067574,5.00827364993925,3.60188760715546));
#32842=CARTESIAN_POINT('Ctrl Pts',(-38.8337120316572,2.66837527862899,5.56202954501839));
#32843=CARTESIAN_POINT('Ctrl Pts',(-38.6944533875744,-0.324816684002235,
6.16042964484212));
#32844=CARTESIAN_POINT('Ctrl Pts',(-38.5551947434915,-3.23848435343815,
5.25058267050353));
#32845=CARTESIAN_POINT('Ctrl Pts',(-38.4159360994087,-5.35927963695485,
3.05524484455452));
#32846=CARTESIAN_POINT('Ctrl Pts',(-38.2766774553258,-6.16797198316708,
0.111896836960587));
#32847=CARTESIAN_POINT('Ctrl Pts',(-38.137418811243,-5.46657067788929,-2.85884667495424));
#32848=CARTESIAN_POINT('Ctrl Pts',(-37.9981601671602,-3.42679855986613,
-5.12966382108567));
#32849=CARTESIAN_POINT('Ctrl Pts',(-37.8589015230773,-0.548049422441559,
-6.14459446325119));
#32850=CARTESIAN_POINT('Ctrl Pts',(-37.7196428789945,2.46487768398001,-5.65515493070466));
#32851=CARTESIAN_POINT('Ctrl Pts',(-37.5803842349116,4.87433315459717,-3.78117383695203));
#32852=CARTESIAN_POINT('Ctrl Pts',(-37.4411255908288,6.09041427589945,-0.98145465263348));
#32853=CARTESIAN_POINT('Ctrl Pts',(-37.301866946746,5.81539006175608,2.05855233523087));
#32854=CARTESIAN_POINT('Ctrl Pts',(-37.1626083026632,4.11659420319502,4.59456760244934));
#32855=CARTESIAN_POINT('Ctrl Pts',(-37.0233496585803,1.40993988013854,6.00570302476329));
#32856=CARTESIAN_POINT('Ctrl Pts',(-36.8840910144975,-1.64190752547249,
5.94647281714569));
#32857=CARTESIAN_POINT('Ctrl Pts',(-36.7448323704146,-4.29176962094978,
4.43137820637648));
#32858=CARTESIAN_POINT('Ctrl Pts',(-36.6055737263319,-5.89088536479951,
1.83135712138482));
#32859=CARTESIAN_POINT('Ctrl Pts',(-36.4663150822489,-6.04774608295902,
-1.21703188261843));
#32860=CARTESIAN_POINT('Ctrl Pts',(-36.3270564381662,-4.72394784374585,
-3.96745712728251));
#32861=CARTESIAN_POINT('Ctrl Pts',(-36.1877977940833,-2.24359382440289,
-5.74653687348798));
#32862=CARTESIAN_POINT('Ctrl Pts',(-36.0485391500005,0.786055295501336,
-6.11870217935716));
#32863=CARTESIAN_POINT('Ctrl Pts',(-35.9092805059176,3.62325589023456,-4.99283647250103));
#32864=CARTESIAN_POINT('Ctrl Pts',(-35.7700218618348,5.57338116547882,-2.64458345898589));
#32865=CARTESIAN_POINT('Ctrl Pts',(-35.6307632177519,6.15898540556072,0.351138236804208));
#32866=CARTESIAN_POINT('Ctrl Pts',(-35.4915045736691,5.23669616202447,3.26089138026614));
#32867=CARTESIAN_POINT('Ctrl Pts',(-35.3522459295863,3.03231587614294,5.37228626513397));
#32868=CARTESIAN_POINT('Ctrl Pts',(-35.2129872855034,0.0855390673244696,
6.16839382296698));
#32869=CARTESIAN_POINT('Ctrl Pts',(-35.0737286414206,-2.88218011977874,
5.45430445101921));
#32870=CARTESIAN_POINT('Ctrl Pts',(-34.9344699973377,-5.14426025514717,
3.40484738491593));
#32871=CARTESIAN_POINT('Ctrl Pts',(-34.7952113532549,-6.14688026746215,
0.521787566678581));
#32872=CARTESIAN_POINT('Ctrl Pts',(-34.6559527091721,-5.64457047567031,
-2.48902057694323));
#32873=CARTESIAN_POINT('Ctrl Pts',(-34.5166940650892,-3.76031049604365,
-4.89044622305572));
#32874=CARTESIAN_POINT('Ctrl Pts',(-34.3774354210064,-0.955420360637483,
-6.09455258585363));
#32875=CARTESIAN_POINT('Ctrl Pts',(-34.2381767769235,2.08338364873574,-5.80654043811255));
#32876=CARTESIAN_POINT('Ctrl Pts',(-34.0989181328408,4.61211653097676,-4.09692328362966));
#32877=CARTESIAN_POINT('Ctrl Pts',(-33.9596594887579,6.0116730952372,-1.38426366103323));
#32878=CARTESIAN_POINT('Ctrl Pts',(-33.820400844675,5.93940238779045,1.66730278089042));
#32879=CARTESIAN_POINT('Ctrl Pts',(-33.6811422005922,4.41299831788288,4.31066643729467));
#32880=CARTESIAN_POINT('Ctrl Pts',(-33.5418835565093,1.80616768928508,5.89865726800925));
#32881=CARTESIAN_POINT('Ctrl Pts',(-33.4026249124266,-1.24286377429694,
6.04249029174199));
#32882=CARTESIAN_POINT('Ctrl Pts',(-33.2633662683437,-3.98760710227222,
4.70695112415288));
#32883=CARTESIAN_POINT('Ctrl Pts',(-33.1241076242609,-5.75607164911629,
2.21901745317509));
#32884=CARTESIAN_POINT('Ctrl Pts',(-32.984848980178,-6.11528737340181,-0.812194328943618));
#32885=CARTESIAN_POINT('Ctrl Pts',(-32.8455903360952,-4.9773081258533,-3.64455801264989));
#32886=CARTESIAN_POINT('Ctrl Pts',(-32.7063316920124,-2.62074334924062,
-5.58463101598189));
#32887=CARTESIAN_POINT('Ctrl Pts',(-32.5670730479295,0.37745337782084,-6.1574287031867));
#32888=CARTESIAN_POINT('Ctrl Pts',(-32.4278144038467,3.28323886320735,-5.22271403145727));
#32889=CARTESIAN_POINT('Ctrl Pts',(-32.2885557597638,5.38519479534925,-3.00933153763413));
#32890=CARTESIAN_POINT('Ctrl Pts',(-32.149297115681,6.16870302787652,-0.0591797357447051));
#32891=CARTESIAN_POINT('Ctrl Pts',(-32.0100384715982,5.44193862853294,2.90546093598537));
#32892=CARTESIAN_POINT('Ctrl Pts',(-31.8707798275153,3.38283403744187,5.15876275500052));
#32893=CARTESIAN_POINT('Ctrl Pts',(-31.7315211834324,0.495516183072966,
6.14905382962034));
#32894=CARTESIAN_POINT('Ctrl Pts',(-31.5922625393497,-2.51311802038301,
5.63388295076159));
#32895=CARTESIAN_POINT('Ctrl Pts',(-31.4530038952668,-4.90646999195102,
3.73937849185396));
#32896=CARTESIAN_POINT('Ctrl Pts',(-31.313745251184,-6.09857960925869,0.929368622662752));
#32897=CARTESIAN_POINT('Ctrl Pts',(-31.1744866071011,-5.79758478702263,
-2.10817691964873));
#32898=CARTESIAN_POINT('Ctrl Pts',(-31.0352279630183,-4.07717755423239,
-4.62958124224203));
#32899=CARTESIAN_POINT('Ctrl Pts',(-30.8959693189355,-1.35856216526917,
-6.01753339254177));
#32900=CARTESIAN_POINT('Ctrl Pts',(-30.7567106748526,1.69266759135437,-5.93222350492919));
#32901=CARTESIAN_POINT('Ctrl Pts',(-30.6174520307698,4.32948454085704,-4.39453784802633));
#32902=CARTESIAN_POINT('Ctrl Pts',(-30.478193386687,5.90632146171901,-1.78094527655773));
#32903=CARTESIAN_POINT('Ctrl Pts',(-30.3389347426041,6.03712416463348,1.26867297127911));
#32904=CARTESIAN_POINT('Ctrl Pts',(-30.1996760985213,4.6898684556178,4.00768426354387));
#32905=CARTESIAN_POINT('Ctrl Pts',(-30.0604174544385,2.19440056268174,5.76550131885839));
#32906=CARTESIAN_POINT('Ctrl Pts',(-29.9211588103556,-0.838318531714867,
6.11176090228006));
#32907=CARTESIAN_POINT('Ctrl Pts',(-29.7819001662728,-3.66579358542456,
4.96168889354382));
#32908=CARTESIAN_POINT('Ctrl Pts',(-29.6426415221899,-5.59577889110529,
2.59685538471367));
#32909=CARTESIAN_POINT('Ctrl Pts',(-29.5033828781071,-6.15575956614548,
-0.403761626537673));
#32910=CARTESIAN_POINT('Ctrl Pts',(-29.3641242340242,-5.20863653411563,
-3.3055263941968));
#32911=CARTESIAN_POINT('Ctrl Pts',(-29.2248655899414,-2.98629224872204,
-5.39800499189085));
#32912=CARTESIAN_POINT('Ctrl Pts',(-29.0856069458586,-0.0328193235427931,
-6.16889959224967));
#32913=CARTESIAN_POINT('Ctrl Pts',(-28.9463483017757,2.92868869846627,-5.42947343623043));
#32914=CARTESIAN_POINT('Ctrl Pts',(-28.8070896576929,5.17317105582995,-3.36075891940781));
#32915=CARTESIAN_POINT('Ctrl Pts',(-28.6678310136101,6.15111511003654,-0.469235751340301));
#32916=CARTESIAN_POINT('Ctrl Pts',(-28.5285723695272,5.62309255113269,2.53716957427995));
#32917=CARTESIAN_POINT('Ctrl Pts',(-28.3893137254444,3.71837820660141,4.92240416868907));
#32918=CARTESIAN_POINT('Ctrl Pts',(-28.2500550813615,0.903299914414111,
6.10249527258116));
#32919=CARTESIAN_POINT('Ctrl Pts',(-28.1107964372787,-2.13293169524463,
5.78852327201652));
#32920=CARTESIAN_POINT('Ctrl Pts',(-27.9715377931959,-4.64696141733948,
4.05735737556035));
#32921=CARTESIAN_POINT('Ctrl Pts',(-27.832279149113,-6.0232838096679,1.33283586215573));
#32922=CARTESIAN_POINT('Ctrl Pts',(-27.6930205050302,-5.92493629964835,
-1.71800149370285));
#32923=CARTESIAN_POINT('Ctrl Pts',(-27.5537618609473,-4.37599713389506,
-4.34822358801822));
#32924=CARTESIAN_POINT('Ctrl Pts',(-27.4145032168645,-1.75569034376417,
-5.91387780598052));
#32925=CARTESIAN_POINT('Ctrl Pts',(-27.2752445727817,1.29445900228884,-6.03164779961905));
#32926=CARTESIAN_POINT('Ctrl Pts',(-27.1359859286988,4.02768824448843,-4.67270015007014));
#32927=CARTESIAN_POINT('Ctrl Pts',(-26.996727284616,5.77482571052857,-2.16974360242729));
#32928=CARTESIAN_POINT('Ctrl Pts',(-26.8574686405332,6.10812283038528,0.864427426787198));
#32929=CARTESIAN_POINT('Ctrl Pts',(-26.7182099964503,4.9459790607797,3.68696222079703));
#32930=CARTESIAN_POINT('Ctrl Pts',(-26.5789513523675,2.57292000159934,5.60682458728878));
#32931=CARTESIAN_POINT('Ctrl Pts',(-26.4396927082847,-0.430062502565925,
6.15397802491548));
#32932=CARTESIAN_POINT('Ctrl Pts',(-26.3004340642018,-3.32775356626403,
5.19446392705473));
#32933=CARTESIAN_POINT('Ctrl Pts',(-26.161175420119,-5.41071662084457,2.96319843010423));
#32934=CARTESIAN_POINT('Ctrl Pts',(-26.0219167760361,-6.16898351249709,
0.00645831205992788));
#32935=CARTESIAN_POINT('Ctrl Pts',(-25.8826581319533,-5.41690910172617,
-2.95186298308237));
#32936=CARTESIAN_POINT('Ctrl Pts',(-25.7433994878705,-3.33862243390558,
-5.18748489453977));
#32937=CARTESIAN_POINT('Ctrl Pts',(-25.6041408437877,-0.442946751361456,
-6.15306407107178));
#32938=CARTESIAN_POINT('Ctrl Pts',(-25.4648821997048,2.56117479945259,-5.61219947381638));
#32939=CARTESIAN_POINT('Ctrl Pts',(-25.325623555622,4.93824846231173,-3.69731002375127));
#32940=CARTESIAN_POINT('Ctrl Pts',(-25.1863649115391,6.10629950432101,-0.877214711906259));
#32941=CARTESIAN_POINT('Ctrl Pts',(-25.0471062674563,5.77935605855753,2.15764752350107));
#32942=CARTESIAN_POINT('Ctrl Pts',(-24.9078476233735,4.03746310953012,4.66425673890698));
#32943=CARTESIAN_POINT('Ctrl Pts',(-24.7685889792906,1.30708522145541,6.02892424161299));
#32944=CARTESIAN_POINT('Ctrl Pts',(-24.6293303352078,-1.74330402533868,
5.91754090501231));
#32945=CARTESIAN_POINT('Ctrl Pts',(-24.490071691125,-4.36688323660318,4.35737651404258));
#32946=CARTESIAN_POINT('Ctrl Pts',(-24.3508130470421,-5.92132616281497,
1.73040335205951));
#32947=CARTESIAN_POINT('Ctrl Pts',(-24.2115544029593,-6.02606129669707,
-1.32022139647321));
#32948=CARTESIAN_POINT('Ctrl Pts',(-24.0722957588764,-4.65544652100326,
-4.04761867983319));
#32949=CARTESIAN_POINT('Ctrl Pts',(-23.9330371147936,-2.14504702264793,
-5.78404465386333));
#32950=CARTESIAN_POINT('Ctrl Pts',(-23.7937784707107,0.890520537411933,
-6.10437322414867));
#32951=CARTESIAN_POINT('Ctrl Pts',(-23.654519826628,3.70806353222781,-4.93017891442268));
#32952=CARTESIAN_POINT('Ctrl Pts',(-23.515261182545,5.61776790283785,-2.54893763695791));
#32953=CARTESIAN_POINT('Ctrl Pts',(-23.3760025384623,6.15208411202769,0.456355525651462));
#32954=CARTESIAN_POINT('Ctrl Pts',(-23.2367438943793,5.18019646906645,3.34991997354075));
#32955=CARTESIAN_POINT('Ctrl Pts',(-23.0974852502966,2.94005050347398,5.42332945009597));
#32956=CARTESIAN_POINT('Ctrl Pts',(-22.9582266062137,-0.0199028173517082,
6.16895478708649));
#32957=CARTESIAN_POINT('Ctrl Pts',(-22.8189679621309,-2.97498336667136,
5.40424585444488));
#32958=CARTESIAN_POINT('Ctrl Pts',(-22.679709318048,-5.2017040097594,3.31642498514721));
#32959=CARTESIAN_POINT('Ctrl Pts',(-22.5404506739652,-6.15490067713796,
0.416649663173528));
#32960=CARTESIAN_POINT('Ctrl Pts',(-22.4011920298824,-5.60120391772031,
-2.58513325756536));
#32961=CARTESIAN_POINT('Ctrl Pts',(-22.2619333857995,-3.67617432800871,
-4.9540025835021));
#32962=CARTESIAN_POINT('Ctrl Pts',(-22.1226747417167,-0.851113491455105,
-6.10999223501298));
#32963=CARTESIAN_POINT('Ctrl Pts',(-21.9834160976338,2.18232395310707,-5.770083314039));
#32964=CARTESIAN_POINT('Ctrl Pts',(-21.8441574535511,4.68146689113202,-4.01749511941093));
#32965=CARTESIAN_POINT('Ctrl Pts',(-21.7048988094681,6.03445458538273,-1.28131071337479));
#32966=CARTESIAN_POINT('Ctrl Pts',(-21.5656401653854,5.91003745606096,1.76857472423761));
#32967=CARTESIAN_POINT('Ctrl Pts',(-21.4263815213025,4.33867632848147,4.38546314588668));
#32968=CARTESIAN_POINT('Ctrl Pts',(-21.2871228772197,1.70508476318431,5.92866639621531));
#32969=CARTESIAN_POINT('Ctrl Pts',(-21.1478642331368,-1.34595968341069,
6.02036475787713));
#32970=CARTESIAN_POINT('Ctrl Pts',(-21.008605589054,-4.06747520564821,4.63810788346854));
#32971=CARTESIAN_POINT('Ctrl Pts',(-20.8693469449712,-5.79315798052477,
2.12031127430337));
#32972=CARTESIAN_POINT('Ctrl Pts',(-20.7300883008883,-6.10051215203808,
-0.91659738712893));
#32973=CARTESIAN_POINT('Ctrl Pts',(-20.5908296568055,-4.9142887429833,-3.72909713440716));
#32974=CARTESIAN_POINT('Ctrl Pts',(-20.4515710127226,-2.52490872870708,
-5.62860863792773));
#32975=CARTESIAN_POINT('Ctrl Pts',(-20.3123123686398,0.482640215683851,
-6.15007786206487));
#32976=CARTESIAN_POINT('Ctrl Pts',(-20.173053724557,3.37202521126839,-5.16583442067456));
#32977=CARTESIAN_POINT('Ctrl Pts',(-20.0337950804741,5.43584324933477,-2.91684889151244));
#32978=CARTESIAN_POINT('Ctrl Pts',(-19.8945364363913,6.16881341654233,0.0462635833377749));
#32979=CARTESIAN_POINT('Ctrl Pts',(-19.7552777923085,5.39148392561755,2.99804942705481));
#32980=CARTESIAN_POINT('Ctrl Pts',(-19.6160191482256,3.29416697845835,5.2158281418477));
#32981=CARTESIAN_POINT('Ctrl Pts',(-19.4767605041428,0.390344966961397,
6.15662489469869));
#32982=CARTESIAN_POINT('Ctrl Pts',(-19.33750186006,-2.60904451113693,5.59010608362329));
#32983=CARTESIAN_POINT('Ctrl Pts',(-19.1982432159771,-4.96966624459001,
3.65497150531144));
#32984=CARTESIAN_POINT('Ctrl Pts',(-19.0589845718943,-6.11357339722781,
0.824996729668839));
#32985=CARTESIAN_POINT('Ctrl Pts',(-18.9197259278114,-5.76070520778121,
-2.20696053347091));
#32986=CARTESIAN_POINT('Ctrl Pts',(-18.7804672837286,-3.99745376981848,
-4.69859155975702));
#32987=CARTESIAN_POINT('Ctrl Pts',(-18.6412086396458,-1.25551280855669,
-6.03987473999303));
#32988=CARTESIAN_POINT('Ctrl Pts',(-18.5019499955629,1.7938131289566,-5.90242608980737));
#32989=CARTESIAN_POINT('Ctrl Pts',(-18.3626913514801,4.40396297659968,-4.31989691867704));
#32990=CARTESIAN_POINT('Ctrl Pts',(-18.2234327073972,5.93589837214893,-1.67973503945581));
#32991=CARTESIAN_POINT('Ctrl Pts',(-18.0841740633144,6.01455828717799,1.37167339312034));
#32992=CARTESIAN_POINT('Ctrl Pts',(-17.9449154192316,4.6206845540694,4.08725745935344));
#32993=CARTESIAN_POINT('Ctrl Pts',(-17.8056567751487,2.09553680906827,5.80216552410355));
#32994=CARTESIAN_POINT('Ctrl Pts',(-17.6663981310659,-0.94265749977486,
6.09653968455664));
#32995=CARTESIAN_POINT('Ctrl Pts',(-17.527139486983,-3.75006264326115,4.89830883661627));
#32996=CARTESIAN_POINT('Ctrl Pts',(-17.3878808429002,-5.63934659460633,
2.50083371561525));
#32997=CARTESIAN_POINT('Ctrl Pts',(-17.2486221988174,-6.14795931166126,
-0.508916092704237));
#32998=CARTESIAN_POINT('Ctrl Pts',(-17.1093635547345,-5.15137804413015,
-3.39406887580522));
#32999=CARTESIAN_POINT('Ctrl Pts',(-16.9701049106517,-2.89359401788095,
-5.44825779005909));
#33000=CARTESIAN_POINT('Ctrl Pts',(-16.8308462665689,0.0726235045509067,
-6.16855940344605));
#33001=CARTESIAN_POINT('Ctrl Pts',(-16.691587622486,3.02106074304649,-5.37862354827693));
#33002=CARTESIAN_POINT('Ctrl Pts',(-16.5523289784032,5.2298570328979,-3.27184882027028));
#33003=CARTESIAN_POINT('Ctrl Pts',(-16.4130703343204,6.15823669226976,-0.364033143049074));
#33004=CARTESIAN_POINT('Ctrl Pts',(-16.2738116902375,5.57890617417189,2.63290812354753));
#33005=CARTESIAN_POINT('Ctrl Pts',(-16.1345530461547,3.63370194282318,4.98523915955686));
#33006=CARTESIAN_POINT('Ctrl Pts',(-15.9952944020718,0.798864903439737,
6.11704292557344));
#33007=CARTESIAN_POINT('Ctrl Pts',(-15.856035757989,-2.23155681472863,5.75122191102848));
#33008=CARTESIAN_POINT('Ctrl Pts',(-15.7167771139061,-4.71563043208565,
3.9773394267077));
#33009=CARTESIAN_POINT('Ctrl Pts',(-15.5775184698233,-6.0451846064719,1.22969197807065));
#33010=CARTESIAN_POINT('Ctrl Pts',(-15.4382598257405,-5.89470694523501,
-1.81901877864247));
#33011=CARTESIAN_POINT('Ctrl Pts',(-15.2990011816577,-4.30103862754144,
-4.42238239093502));
#33012=CARTESIAN_POINT('Ctrl Pts',(-15.1597425375748,-1.65435464376045,
-5.9430219585598));
#33013=CARTESIAN_POINT('Ctrl Pts',(-15.020483893492,1.39736205606941,-6.00864199062594));
#33014=CARTESIAN_POINT('Ctrl Pts',(-14.8812252494091,4.10696507972471,-4.60317685095605));
#33015=CARTESIAN_POINT('Ctrl Pts',(-14.7419666053263,5.81106712012186,-2.07072407932459));
#33016=CARTESIAN_POINT('Ctrl Pts',(-14.6027079612435,6.09245589424167,0.968700399491914));
#33017=CARTESIAN_POINT('Ctrl Pts',(-14.4634493171606,4.88223948711466,3.77095967595971));
#33018=CARTESIAN_POINT('Ctrl Pts',(-14.3241906730778,2.47671303729191,5.64998157679864));
#33019=CARTESIAN_POINT('Ctrl Pts',(-14.1849320289949,-0.53518267691531,
6.14572849950156));
#33020=CARTESIAN_POINT('Ctrl Pts',(-14.0456733849121,-3.41605056463389,
5.13682760340662));
#33021=CARTESIAN_POINT('Ctrl Pts',(-13.9064147408293,-5.46057284557919,
2.87028630721381));
#33022=CARTESIAN_POINT('Ctrl Pts',(-13.7671560967464,-6.16819275243593,
-0.0989820996583846));
#33023=CARTESIAN_POINT('Ctrl Pts',(-13.6278974526636,-5.36566495725375,
-3.04401689445949));
#33024=CARTESIAN_POINT('Ctrl Pts',(-13.4886388085808,-3.24947091811263,
-5.24379042674249));
#33025=CARTESIAN_POINT('Ctrl Pts',(-13.3493801644979,-0.337714671890257,
-6.15973604041975));
#33026=CARTESIAN_POINT('Ctrl Pts',(-13.2101215204151,2.65672365904785,-5.56760439387636));
#33027=CARTESIAN_POINT('Ctrl Pts',(-13.0708628763323,5.00072104404122,-3.61236602892606));
#33028=CARTESIAN_POINT('Ctrl Pts',(-12.9316042322494,6.12040075669628,-0.772718489935025));
#33029=CARTESIAN_POINT('Ctrl Pts',(-12.7923455881666,5.74163359694582,2.25611234775199));
#33030=CARTESIAN_POINT('Ctrl Pts',(-12.6530869440838,3.95715245736665,4.73258319698796));
#33031=CARTESIAN_POINT('Ctrl Pts',(-12.5138283000009,1.20384869340539,6.05038408786103));
#33032=CARTESIAN_POINT('Ctrl Pts',(-12.3745696559181,-1.84419121303957,
5.88688016329563));
#33033=CARTESIAN_POINT('Ctrl Pts',(-12.2353110118352,-4.4407210525541,4.28210179942731));
#33034=CARTESIAN_POINT('Ctrl Pts',(-12.0960523677524,-5.95003702537131,
1.62894403954418));
#33035=CARTESIAN_POINT('Ctrl Pts',(-11.9567937236695,-6.00261597625248,
-1.42302520318319));
#33036=CARTESIAN_POINT('Ctrl Pts',(-11.8175350795867,-4.58558509381898,
-4.12659770690106));
#33037=CARTESIAN_POINT('Ctrl Pts',(-11.6782764355039,-2.04587353815267,
-5.81986260603654));
#33038=CARTESIAN_POINT('Ctrl Pts',(-11.539017791421,0.994725610736604,-6.08826085566316));
#33039=CARTESIAN_POINT('Ctrl Pts',(-11.3997591473382,3.7917878509228,-4.86608098790496));
#33040=CARTESIAN_POINT('Ctrl Pts',(-11.2605005032553,5.66051339030982,-2.45254713418094));
#33041=CARTESIAN_POINT('Ctrl Pts',(-11.1212418591725,6.1433854663204,0.561439488688986));
#33042=CARTESIAN_POINT('Ctrl Pts',(-10.9819832150897,5.12218336419516,3.43796987636866));
#33043=CARTESIAN_POINT('Ctrl Pts',(-10.8427245710069,2.84692618510974,5.47278819102222));
#33044=CARTESIAN_POINT('Ctrl Pts',(-10.703465926924,-0.125338887352521,
6.16771347020701));
#33045=CARTESIAN_POINT('Ctrl Pts',(-10.5642072828412,-3.06691746211474,
5.35260838917175));
#33046=CARTESIAN_POINT('Ctrl Pts',(-10.4249486387583,-5.2576280689577,3.22703368060576));
#33047=CARTESIAN_POINT('Ctrl Pts',(-10.2856899946755,-6.16112291177051,
0.311390034060484));
#33048=CARTESIAN_POINT('Ctrl Pts',(-10.1464313505927,-5.55620094910737,
-2.68049068276575));
#33049=CARTESIAN_POINT('Ctrl Pts',(-10.0071727065098,-3.59096415321422,
-5.01611161534373));
#33050=CARTESIAN_POINT('Ctrl Pts',(-9.86791406242698,-0.746557966588395,
-6.12364682928231));
#33051=CARTESIAN_POINT('Ctrl Pts',(-9.72865541834415,2.28062668415683,-5.73194044061589));
#33052=CARTESIAN_POINT('Ctrl Pts',(-9.58939677426131,4.74944954490643,-3.93689323040948));
#33053=CARTESIAN_POINT('Ctrl Pts',(-9.45013813017848,6.05547308921799,-1.17798342645918));
#33054=CARTESIAN_POINT('Ctrl Pts',(-9.31087948609562,5.87894588690616,1.86932997249951));
#33055=CARTESIAN_POINT('Ctrl Pts',(-9.17162084201281,4.26308678012096,4.45897862659307));
#33056=CARTESIAN_POINT('Ctrl Pts',(-9.03236219792997,1.60350369080462,5.95694344448826));
#33057=CARTESIAN_POINT('Ctrl Pts',(-8.89310355384712,-1.44866236585221,
5.99648035409267));
#33058=CARTESIAN_POINT('Ctrl Pts',(-8.7538449097643,-4.14615498239031,4.56790960388402));
#33059=CARTESIAN_POINT('Ctrl Pts',(-8.61458626568144,-5.82855182124194,
2.02098563932378));
#33060=CARTESIAN_POINT('Ctrl Pts',(-8.47532762159861,-6.08395464542259,
-1.02073265828857));
#33061=CARTESIAN_POINT('Ctrl Pts',(-8.33606897751578,-4.84983363404122,
-3.81254678782812));
#33062=CARTESIAN_POINT('Ctrl Pts',(-8.19681033343293,-2.42833644755147,
-5.67094184282902));
#33063=CARTESIAN_POINT('Ctrl Pts',(-8.05755168935011,0.587686048575971,
-6.14093025490153));
#33064=CARTESIAN_POINT('Ctrl Pts',(-7.91829304526725,3.45982641076282,-5.10744559389954));
#33065=CARTESIAN_POINT('Ctrl Pts',(-7.77903440118443,5.48490360333593,-2.82351407812473));
#33066=CARTESIAN_POINT('Ctrl Pts',(-7.63977575710159,6.16712156551101,0.151693386358204));
#33067=CARTESIAN_POINT('Ctrl Pts',(-7.50051711301874,5.33945408244398,3.08976202784748));
#33068=CARTESIAN_POINT('Ctrl Pts',(-7.36125846893593,3.20453751745409,5.27136970686795));
#33069=CARTESIAN_POINT('Ctrl Pts',(-7.22199982485307,0.2850597102479,6.1623972809978));
#33070=CARTESIAN_POINT('Ctrl Pts',(-7.08274118077024,-2.70420876071548,
5.54469604809187));
#33071=CARTESIAN_POINT('Ctrl Pts',(-6.94348253668739,-5.0314105924327,3.56949670648567));
#33072=CARTESIAN_POINT('Ctrl Pts',(-6.80422389260456,-6.12678108405827,
0.720383811090751));
#33073=CARTESIAN_POINT('Ctrl Pts',(-6.66496524852172,-5.72214261903566,
-2.30509937631144));
#33074=CARTESIAN_POINT('Ctrl Pts',(-6.52570660443889,-3.91656211576974,
-4.76622916786142));
#33075=CARTESIAN_POINT('Ctrl Pts',(-6.38644796035605,-1.15209664953208,
-6.06045151761753));
#33076=CARTESIAN_POINT('Ctrl Pts',(-6.24718931627322,1.89443459798825,-5.87090426094661));
#33077=CARTESIAN_POINT('Ctrl Pts',(-6.10793067219037,4.47715477966845,-4.24399391683683));
#33078=CARTESIAN_POINT('Ctrl Pts',(-5.96867202810754,5.96374108979948,-1.57803406208271));
#33079=CARTESIAN_POINT('Ctrl Pts',(-5.82941338402469,5.99023523618298,1.47427307594201));
#33080=CARTESIAN_POINT('Ctrl Pts',(-5.69015473994186,4.55015070390546,4.16563654907681));
#33081=CARTESIAN_POINT('Ctrl Pts',(-5.55089609585903,1.99606083729069,5.8371346070731));
#33082=CARTESIAN_POINT('Ctrl Pts',(-5.41163745177617,-1.0467210672592,6.07953734215126));
#33083=CARTESIAN_POINT('Ctrl Pts',(-5.27237880769334,-3.83323610761724,
4.83349772220027));
#33084=CARTESIAN_POINT('Ctrl Pts',(-5.13312016361051,-5.6812667439325,2.4040814194911));
#33085=CARTESIAN_POINT('Ctrl Pts',(-4.99386151952768,-6.1383629100772,-0.613921877313705));
#33086=CARTESIAN_POINT('Ctrl Pts',(-4.85460287544483,-5.09261456163162,
-3.4816197687159));
#33087=CARTESIAN_POINT('Ctrl Pts',(-4.71534423136201,-2.80005041376394,
-5.49691886129279));
#33088=CARTESIAN_POINT('Ctrl Pts',(-4.57608558727915,0.178045115442175,
-6.16641704915611));
#33089=CARTESIAN_POINT('Ctrl Pts',(-4.43682694319632,3.11255017451608,-5.32620227726806));
#33090=CARTESIAN_POINT('Ctrl Pts',(-4.29756829911348,5.28501508955106,-3.18198283943735));
#33091=CARTESIAN_POINT('Ctrl Pts',(-4.15830965503065,6.16355912483164,-0.258724181243916));
#33092=CARTESIAN_POINT('Ctrl Pts',(-4.01905101094781,5.53308990090931,2.72787745980472));
#33093=CARTESIAN_POINT('Ctrl Pts',(-3.87979236686497,3.54796408073617,5.04661769594891));
#33094=CARTESIAN_POINT('Ctrl Pts',(-3.74053372278214,0.694196501382891,
6.12980346379193));
#33095=CARTESIAN_POINT('Ctrl Pts',(-3.60127507869929,-2.32952997734448,
5.71224031111489));
#33096=CARTESIAN_POINT('Ctrl Pts',(-3.46201643461646,-4.78292175945639,
3.89615948469104));
#33097=CARTESIAN_POINT('Ctrl Pts',(-3.32275779053362,-6.06531928215492,
1.12618883532147));
#33098=CARTESIAN_POINT('Ctrl Pts',(-3.18349914645078,-5.86275543225447,
-1.91950463110544));
#33099=CARTESIAN_POINT('Ctrl Pts',(-3.04424050236794,-4.22482355821538,
-4.49524917986447));
#33100=CARTESIAN_POINT('Ctrl Pts',(-2.90498185828511,-1.55253561844441,
-5.97042983721744));
#33101=CARTESIAN_POINT('Ctrl Pts',(-2.76572321420226,1.4998568657823,-5.98388073648606));
#33102=CARTESIAN_POINT('Ctrl Pts',(-2.62646457011943,4.18504205126321,-4.53230871830385));
#33103=CARTESIAN_POINT('Ctrl Pts',(-2.4872059260366,5.84561080673752,-1.97109958690181));
#33104=CARTESIAN_POINT('Ctrl Pts',(-2.34794728195376,6.07500902664705,1.07269036255581));
#33105=CARTESIAN_POINT('Ctrl Pts',(-2.20868863787092,4.81707355040727,3.85385543356388));
#33106=CARTESIAN_POINT('Ctrl Pts',(-2.06942999378809,2.37978249342083,5.69148790301832));
#33107=CARTESIAN_POINT('Ctrl Pts',(-1.93017134970525,-0.640146496858891,
6.13568348276358));
#33108=CARTESIAN_POINT('Ctrl Pts',(-1.7909127056224,-3.50334955028659,5.07769053033222));
#33109=CARTESIAN_POINT('Ctrl Pts',(-1.65165406153957,-5.50883374938536,
2.77653563583237));
#33110=CARTESIAN_POINT('Ctrl Pts',(-1.51239541745673,-6.16559992641659,
-0.204393623380619));
#33111=CARTESIAN_POINT('Ctrl Pts',(-1.37313677337389,-5.3128532304277,-3.13528142757007));
#33112=CARTESIAN_POINT('Ctrl Pts',(-1.23387812929106,-3.159370029524,-5.29856408183426));
#33113=CARTESIAN_POINT('Ctrl Pts',(-1.09461948520822,-0.232383984270165,
-6.16460819970066));
#33114=CARTESIAN_POINT('Ctrl Pts',(-0.955360841125374,2.75149645773078,
-5.52138315322195));
#33115=CARTESIAN_POINT('Ctrl Pts',(-0.816102197042544,5.06173243386037,
-3.52636582309806));
#33116=CARTESIAN_POINT('Ctrl Pts',(-0.676843552959711,6.13271433141243,
-0.66799816598022));
#33117=CARTESIAN_POINT('Ctrl Pts',(-0.537584908876864,5.70223288207738,
2.35392126034556));
#33118=CARTESIAN_POINT('Ctrl Pts',(-0.398326264794022,3.87568730064295,
4.7995207354176));
#33119=CARTESIAN_POINT('Ctrl Pts',(-0.259067620711194,1.10025735360832,
6.07008854307166));
#33120=CARTESIAN_POINT('Ctrl Pts',(-0.119808976628351,-1.9445335606143,
5.85447565379037));
#33121=CARTESIAN_POINT('Ctrl Pts',(0.0194496674544829,-4.51327330568083,
4.20562269082728));
#33122=CARTESIAN_POINT('Ctrl Pts',(0.158708311537311,-5.97698652079983,
1.52691759668036));
#33123=CARTESIAN_POINT('Ctrl Pts',(0.297966955620161,-5.97746201560441,
-1.52523260608557));
#33124=CARTESIAN_POINT('Ctrl Pts',(0.437225599703,-4.51429511200085,-4.20475193064767));
#33125=CARTESIAN_POINT('Ctrl Pts',(0.530064695758222,-2.80228789376692,
-5.30353925874901));
#33126=CARTESIAN_POINT('Ctrl Pts',(0.576484243785833,-1.8665303149515,-5.61462333072015));
#33127=CARTESIAN_POINT('',(-8.88178419700125E-15,-4.03672702691112,4.32582540941094));
#33128=CARTESIAN_POINT('Ctrl Pts',(-1.02140518265514E-14,-4.03701234814588,
4.32595897371309));
#33129=CARTESIAN_POINT('Ctrl Pts',(-9.9843844026724E-15,-4.1299458592561,
4.22407952174816));
#33130=CARTESIAN_POINT('Ctrl Pts',(-5.92110397111577E-15,-4.21916354543406,
4.11905201329014));
#33131=CARTESIAN_POINT('Ctrl Pts',(-3.33066907387547E-15,-4.30445389140253,
4.01101265725413));
#33132=CARTESIAN_POINT('Ctrl Pts',(-9.4273941981131E-17,-4.40735712598554,
3.88066262675386));
#33133=CARTESIAN_POINT('Ctrl Pts',(-1.51545993841484E-15,-4.50454492550802,
3.74592848472362));
#33134=CARTESIAN_POINT('Ctrl Pts',(3.33066907387547E-16,-4.59581941741086,
3.60722779298289));
#33135=CARTESIAN_POINT('Ctrl Pts',(2.17437774338676E-15,-4.68673760524928,
3.46906854079636));
#33136=CARTESIAN_POINT('Ctrl Pts',(8.54816426306082E-15,-4.77178878425916,
3.3269729018291));
#33137=CARTESIAN_POINT('Ctrl Pts',(6.10622663543836E-15,-4.85072810092883,
3.18133880832367));
#33138=CARTESIAN_POINT('Ctrl Pts',(5.53956788225534E-15,-4.86904619974314,
3.14754399189869));
#33139=CARTESIAN_POINT('Ctrl Pts',(1.2664160508966E-15,-4.88703496548394,
3.11355859884732));
#33140=CARTESIAN_POINT('Ctrl Pts',(2.22044604925031E-16,-4.90469093726253,
3.07938755292361));
#33141=CARTESIAN_POINT('Ctrl Pts',(-4.42079666650615E-16,-4.91591851289345,
3.05765790771874));
#33142=CARTESIAN_POINT('Ctrl Pts',(1.71356643288325E-14,-4.92701076494171,
3.03585452116636));
#33143=CARTESIAN_POINT('Ctrl Pts',(1.69864122767649E-14,-4.9379615767523,
3.01398949575384));
#33144=CARTESIAN_POINT('Ctrl Pts',(1.5989203206649E-14,-5.01112806733903,
2.86790104097132));
#33145=CARTESIAN_POINT('Ctrl Pts',(9.31012957414554E-15,-5.07805250460248,
2.71893170034809));
#33146=CARTESIAN_POINT('Ctrl Pts',(4.55191440096314E-15,-5.13854422193342,
2.56748287243489));
#33147=CARTESIAN_POINT('Ctrl Pts',(-1.71363691774166E-16,-5.19859178028505,
2.41714605389738));
#33148=CARTESIAN_POINT('Ctrl Pts',(-4.82591573396116E-15,-5.25230089977517,
2.26436530798515));
#33149=CARTESIAN_POINT('Ctrl Pts',(-4.05231403988182E-15,-5.29943494362445,
2.10952414416537));
#33150=CARTESIAN_POINT('Ctrl Pts',(-3.46892256503307E-15,-5.33497984944261,
1.99275473218054));
#33151=CARTESIAN_POINT('Ctrl Pts',(7.69623986356005E-15,-5.36678449339774,
1.87481330294842));
#33152=CARTESIAN_POINT('Ctrl Pts',(9.6034291630076E-15,-5.39472742260068,
1.75586454471506));
#33153=CARTESIAN_POINT('Ctrl Pts',(1.01947903236083E-14,-5.40339167163397,
1.71898216720734));
#33154=CARTESIAN_POINT('Ctrl Pts',(6.937645723431E-15,-5.41168451537563,
1.68200295496824));
#33155=CARTESIAN_POINT('Ctrl Pts',(7.04991620636974E-15,-5.41960198349953,
1.64493186461997));
#33156=CARTESIAN_POINT('Ctrl Pts',(7.11459518622115E-15,-5.42416323368618,
1.62357522445113));
#33157=CARTESIAN_POINT('Ctrl Pts',(-1.68019455085037E-14,-5.42859776171347,
1.60219807679196));
#33158=CARTESIAN_POINT('Ctrl Pts',(-1.63757896132211E-14,-5.43290502002547,
1.58080206259592));
#33159=CARTESIAN_POINT('Ctrl Pts',(-1.51559929927354E-14,-5.44523379264295,
1.51955971889707));
#33160=CARTESIAN_POINT('Ctrl Pts',(4.59923465264813E-15,-5.45652033974346,
1.45816097348265));
#33161=CARTESIAN_POINT('Ctrl Pts',(4.38538094726937E-15,-5.46675441513566,
1.39662819681779));
#33162=CARTESIAN_POINT('Ctrl Pts',(3.83850247844808E-15,-5.49288327644095,
1.23952740113381));
#33163=CARTESIAN_POINT('Ctrl Pts',(2.01620486307756E-14,-5.51215540965326,
1.08155306540347));
#33164=CARTESIAN_POINT('Ctrl Pts',(1.94844140821715E-14,-5.52463713258762,
0.923142281064311));
#33165=CARTESIAN_POINT('Ctrl Pts',(1.88042532098635E-14,-5.53716538926583,
0.764140917451617));
#33166=CARTESIAN_POINT('Ctrl Pts',(4.56756685228552E-15,-5.54285239098084,
0.604699060344447));
#33167=CARTESIAN_POINT('Ctrl Pts',(2.66453525910038E-15,-5.54171302337198,
0.445262773869298));
#33168=CARTESIAN_POINT('Ctrl Pts',(7.86960708762468E-16,-5.54058889719691,
0.287959282451643));
#33169=CARTESIAN_POINT('Ctrl Pts',(4.79544066007618E-15,-5.53281957145188,
0.130660511512922));
#33170=CARTESIAN_POINT('Ctrl Pts',(4.71844785465692E-15,-5.51837155975906,
-0.0261901709885422));
#33171=CARTESIAN_POINT('Ctrl Pts',(4.66374349800356E-15,-5.50810606572656,
-0.137634553748184));
#33172=CARTESIAN_POINT('Ctrl Pts',(-4.94803098190201E-15,-5.4944679918248,
-0.248852439276699));
#33173=CARTESIAN_POINT('Ctrl Pts',(-6.82787160144471E-15,-5.47743131033041,
-0.359677207278218));
#33174=CARTESIAN_POINT('Ctrl Pts',(-7.48657969095659E-15,-5.47146154895696,
-0.398510909689988));
#33175=CARTESIAN_POINT('Ctrl Pts',(1.73538460866958E-14,-5.46507438832126,
-0.437296275458263));
#33176=CARTESIAN_POINT('Ctrl Pts',(1.80966353013901E-14,-5.45826837936944,
-0.476025900372521));
#33177=CARTESIAN_POINT('Ctrl Pts',(1.85346830350253E-14,-5.45425464742845,
-0.498866060249126));
#33178=CARTESIAN_POINT('Ctrl Pts',(-7.23173250167379E-15,-5.45009491258204,
-0.521688207844201));
#33179=CARTESIAN_POINT('Ctrl Pts',(-6.77236045021345E-15,-5.44579287453235,
-0.544470609171142));
#33180=CARTESIAN_POINT('Ctrl Pts',(-3.69376219740839E-15,-5.41696167598384,
-0.697152646959159));
#33181=CARTESIAN_POINT('Ctrl Pts',(-6.13749631345723E-15,-5.38170771746027,
-0.848259769607838));
#33182=CARTESIAN_POINT('Ctrl Pts',(-3.83026943495679E-15,-5.34006209286253,
-0.997382404033546));
#33183=CARTESIAN_POINT('Ctrl Pts',(-2.06755517157137E-15,-5.30824496331619,
-1.11131163966496));
#33184=CARTESIAN_POINT('Ctrl Pts',(-6.3369974246489E-15,-5.27269602122346,
-1.22408245652815));
#33185=CARTESIAN_POINT('Ctrl Pts',(-4.27435864480685E-15,-5.23340997239925,
-1.33550483482684));
#33186=CARTESIAN_POINT('Ctrl Pts',(-1.56325154693959E-15,-5.18177287197461,
-1.48195704139786));
#33187=CARTESIAN_POINT('Ctrl Pts',(1.51022923062233E-14,-5.12368063549572,
-1.62608107617323));
#33188=CARTESIAN_POINT('Ctrl Pts',(1.29340982368831E-14,-5.05935921644069,
-1.76748797034581));
#33189=CARTESIAN_POINT('Ctrl Pts',(1.07809790568834E-14,-4.9954850074801,
-1.90791169916812));
#33190=CARTESIAN_POINT('Ctrl Pts',(4.29962680979437E-15,-4.92546739796093,
-2.04565651048916));
#33191=CARTESIAN_POINT('Ctrl Pts',(6.41153796721028E-15,-4.84949146114621,
-2.18030540628267));
#33192=CARTESIAN_POINT('Ctrl Pts',(7.393084765491E-15,-4.81418034625153,
-2.24288578145331));
#33193=CARTESIAN_POINT('Ctrl Pts',(1.40120518047632E-14,-4.77758171885201,
-2.30479684864787));
#33194=CARTESIAN_POINT('Ctrl Pts',(1.40998324127395E-14,-4.73971195737352,
-2.36599353753954));
#33195=CARTESIAN_POINT('Ctrl Pts',(1.41270155954857E-14,-4.72798475850173,
-2.38494442904003));
#33196=CARTESIAN_POINT('Ctrl Pts',(1.3925834722576E-14,-4.71613565303999,
-2.40382679808695));
#33197=CARTESIAN_POINT('Ctrl Pts',(1.42663658664333E-14,-4.70416510366087,
-2.42263926232305));
#33198=CARTESIAN_POINT('Ctrl Pts',(1.45308547402812E-14,-4.69486763650776,
-2.43725081128081));
#33199=CARTESIAN_POINT('Ctrl Pts',(-1.62837640444609E-16,-4.68549762532919,
-2.45181900290397));
#33200=CARTESIAN_POINT('Ctrl Pts',(2.77555756156289E-17,-4.67606063554748,
-2.46633519301188));
#33201=CARTESIAN_POINT('Ctrl Pts',(1.69856282096252E-15,-4.59333266008503,
-2.59358922706657));
#33202=CARTESIAN_POINT('Ctrl Pts',(-4.00822838861647E-15,-4.50535159703235,
-2.71702212155416));
#33203=CARTESIAN_POINT('Ctrl Pts',(-2.08166817117217E-15,-4.41235800541746,
-2.83629106116441));
#33204=CARTESIAN_POINT('Ctrl Pts',(-9.83010432275142E-17,-4.31662238757981,
-2.95907678676274));
#33205=CARTESIAN_POINT('Ctrl Pts',(5.58857198077528E-15,-4.21557390510044,
-3.07745022281706));
#33206=CARTESIAN_POINT('Ctrl Pts',(3.91353616180368E-15,-4.10943425467638,
-3.19099631382378));
#33207=CARTESIAN_POINT('Ctrl Pts',(2.23850034283208E-15,-4.00329460425232,
-3.3045424048305));
#33208=CARTESIAN_POINT('Ctrl Pts',(3.87429654806338E-15,-3.89206320923292,
-3.41326181578148));
#33209=CARTESIAN_POINT('Ctrl Pts',(3.13638004456607E-15,-3.77592911856888,
-3.51668791312134));
#33210=CARTESIAN_POINT('Ctrl Pts',(2.66650929863803E-15,-3.69724273478636,
-3.58676402550038));
#33211=CARTESIAN_POINT('Ctrl Pts',(8.72292990203801E-15,-3.61630486923059,
-3.65440893269852));
#33212=CARTESIAN_POINT('Ctrl Pts',(8.90953977261688E-15,-3.5332392463504,
-3.71953115971285));
#33213=CARTESIAN_POINT('Ctrl Pts',(9.00727170106557E-15,-3.48973584812881,
-3.75363718428294));
#33214=CARTESIAN_POINT('Ctrl Pts',(1.35643768055353E-14,-3.44564878417463,
-3.78705107374077));
#33215=CARTESIAN_POINT('Ctrl Pts',(1.31838984174237E-14,-3.40099558655679,
-3.81975833303289));
#33216=CARTESIAN_POINT('Ctrl Pts',(1.29459073673587E-14,-3.37306479804978,
-3.84021688002767));
#33217=CARTESIAN_POINT('Ctrl Pts',(-1.02962754854352E-14,-3.34491250359703,
-3.86039893481383));
#33218=CARTESIAN_POINT('Ctrl Pts',(-1.092181900475E-14,-3.31654297785117,
-3.88030075778515));
#33219=CARTESIAN_POINT('Ctrl Pts',(-1.12805760383569E-14,-3.30027269994537,
-3.89171470222243));
#33220=CARTESIAN_POINT('Ctrl Pts',(-1.25188543466211E-14,-3.28393878107512,
-3.90303097900495));
#33221=CARTESIAN_POINT('Ctrl Pts',(-1.23095977855314E-14,-3.26754449164669,
-3.9142476194029));
#33222=CARTESIAN_POINT('Ctrl Pts',(-1.07581489276142E-14,-3.14599560697777,
-3.99740890163195));
#33223=CARTESIAN_POINT('Ctrl Pts',(-1.38744807549176E-15,-3.02108905880586,
-4.07512598255334));
#33224=CARTESIAN_POINT('Ctrl Pts',(-2.26207941267376E-15,-2.89320350651368,
-4.1472297958351));
#33225=CARTESIAN_POINT('Ctrl Pts',(-3.13634849819265E-15,-2.76537092139982,
-4.21930374541867));
#33226=CARTESIAN_POINT('Ctrl Pts',(2.21681871676629E-15,-2.63456105055413,
-4.2857693370254));
#33227=CARTESIAN_POINT('Ctrl Pts',(1.25593979660721E-15,-2.50113319349224,
-4.34640974797566));
#33228=CARTESIAN_POINT('Ctrl Pts',(3.04280062723563E-16,-2.3689855146534,
-4.40646834239041));
#33229=CARTESIAN_POINT('Ctrl Pts',(6.54382616372687E-15,-2.23426913139978,
-4.46081317271807));
#33230=CARTESIAN_POINT('Ctrl Pts',(4.03843625207401E-15,-2.09732548174527,
-4.50918342436963));
#33231=CARTESIAN_POINT('Ctrl Pts',(1.58747746198249E-15,-1.96335701627535,
-4.55650280284757));
#33232=CARTESIAN_POINT('Ctrl Pts',(4.96478138896302E-15,-1.82725639023716,
-4.59810443322033));
#33233=CARTESIAN_POINT('Ctrl Pts',(5.59968738045313E-15,-1.68934572884667,
-4.63369442980763));
#33234=CARTESIAN_POINT('Ctrl Pts',(5.81026669552682E-15,-1.64360489003554,
-4.64549856649129));
#33235=CARTESIAN_POINT('Ctrl Pts',(-8.97215586048935E-17,-1.59766499830972,
-4.65664097727771));
#33236=CARTESIAN_POINT('Ctrl Pts',(-2.77555756156289E-17,-1.55153804394499,
-4.66710967952236));
#33237=CARTESIAN_POINT('Ctrl Pts',(-1.52162519220488,-5.91720137462112,
-6.73836950611244E-5));
#33238=CARTESIAN_POINT('Ctrl Pts',(-1.51854860062216,-5.9172390196691,-0.0654090771404739));
#33239=CARTESIAN_POINT('Ctrl Pts',(-1.51547200903945,-5.91617931145235,
-0.13074954736745));
#33240=CARTESIAN_POINT('Ctrl Pts',(-1.51239541745673,-5.9140144475799,-0.196053380876696));
#33241=CARTESIAN_POINT('Ctrl Pts',(-1.46597586942912,-5.88135102775363,
-1.1813562247771));
#33242=CARTESIAN_POINT('Ctrl Pts',(-1.41955632140151,-5.59710212909066,
-2.15831882617359));
#33243=CARTESIAN_POINT('Ctrl Pts',(-1.3731367733739,-5.0960638129419,-3.00734723591585));
#33244=CARTESIAN_POINT('Ctrl Pts',(-1.32671722534628,-4.59502549679315,
-3.85637564565811));
#33245=CARTESIAN_POINT('Ctrl Pts',(-1.28029767731867,-3.87719776315859,
-4.57746986374617));
#33246=CARTESIAN_POINT('Ctrl Pts',(-1.23387812929106,-3.03045288879903,
-5.08235765910126));
#33247=CARTESIAN_POINT('Ctrl Pts',(-1.18745858126345,-2.18370801443943,
-5.58724545445638));
#33248=CARTESIAN_POINT('Ctrl Pts',(-1.14103903323584,-1.20804599935479,
-5.87592682707852));
#33249=CARTESIAN_POINT('Ctrl Pts',(-1.09461948520822,-0.222901584812313,
-5.91306333897647));
#33250=CARTESIAN_POINT('Ctrl Pts',(-1.04819993718061,0.762242829730162,
-5.95019985087442));
#33251=CARTESIAN_POINT('Ctrl Pts',(-1.00178038915299,1.75686964373051,-5.73579150204818));
#33252=CARTESIAN_POINT('Ctrl Pts',(-0.955360841125374,2.63922238008561,
-5.29608443928106));
#33253=CARTESIAN_POINT('Ctrl Pts',(-0.90894129309776,3.52157511644072,-4.85637737651394));
#33254=CARTESIAN_POINT('Ctrl Pts',(-0.862521745070147,4.29165377515062,
-4.19137159980593));
#33255=CARTESIAN_POINT('Ctrl Pts',(-0.816102197042535,4.85519008743088,
-3.38247410193227));
#33256=CARTESIAN_POINT('Ctrl Pts',(-0.769682649014926,5.41872639971112,
-2.57357660405865));
#33257=CARTESIAN_POINT('Ctrl Pts',(-0.723263100987323,5.77572036556173,
-1.62078738501953));
#33258=CARTESIAN_POINT('Ctrl Pts',(-0.676843552959712,5.88247044026457,
-0.640739537778962));
#33259=CARTESIAN_POINT('Ctrl Pts',(-0.630424004932098,5.98922051496742,
0.339308309461658));
#33260=CARTESIAN_POINT('Ctrl Pts',(-0.58400445690448,5.84572669852239,1.34661478490362));
#33261=CARTESIAN_POINT('Ctrl Pts',(-0.537584908876865,5.46955552672748,
2.2578679351366));
#33262=CARTESIAN_POINT('Ctrl Pts',(-0.49116536084925,5.09338435493256,3.16912108536958));
#33263=CARTESIAN_POINT('Ctrl Pts',(-0.444745812821634,4.48453582778773,
3.98432091039362));
#33264=CARTESIAN_POINT('Ctrl Pts',(-0.398326264794021,3.7175399063762,4.60368212418131));
#33265=CARTESIAN_POINT('Ctrl Pts',(-0.351906716766411,2.95054398496471,
5.22304333796897));
#33266=CARTESIAN_POINT('Ctrl Pts',(-0.305487168738803,2.02540066928651,
5.64656594052032));
#33267=CARTESIAN_POINT('Ctrl Pts',(-0.259067620711191,1.05536385907698,
5.82239176024911));
#33268=CARTESIAN_POINT('Ctrl Pts',(-0.21264807268358,0.085327048867453,
5.9982175799779));
#33269=CARTESIAN_POINT('Ctrl Pts',(-0.166228524655965,-0.929603255873433,
5.92634661688413));
#33270=CARTESIAN_POINT('Ctrl Pts',(-0.119808976628353,-1.86519169908829,
5.61560230817674));
#33271=CARTESIAN_POINT('Ctrl Pts',(-0.0798726510855764,-2.67011045056044,
5.34825834641043));
#33272=CARTESIAN_POINT('Ctrl Pts',(-0.0399363255428003,-3.41630234235058,
4.90410631410206));
#33273=CARTESIAN_POINT('Ctrl Pts',(-2.60208521396521E-14,-4.03701234814564,
4.32595897371332));
#33274=CARTESIAN_POINT('',(-59.58325,-2.85728527160914,-4.0034352877952));
#33275=CARTESIAN_POINT('Ctrl Pts',(-59.58325,-2.85728527160908,-4.00343528779524));
#33276=CARTESIAN_POINT('Ctrl Pts',(-59.58325,-2.95747118827891,-3.9459219613317));
#33277=CARTESIAN_POINT('Ctrl Pts',(-59.58325,-3.0554882232272,-3.88491300663017));
#33278=CARTESIAN_POINT('Ctrl Pts',(-59.58325,-3.15114152320849,-3.82051500336858));
#33279=CARTESIAN_POINT('Ctrl Pts',(-59.58325,-3.27116313425674,-3.7397111826822));
#33280=CARTESIAN_POINT('Ctrl Pts',(-59.58325,-3.38746433751411,-3.65357321571129));
#33281=CARTESIAN_POINT('Ctrl Pts',(-59.58325,-3.49982428652864,-3.56247863507039));
#33282=CARTESIAN_POINT('Ctrl Pts',(-59.58325,-3.57206065704153,-3.50391380003259));
#33283=CARTESIAN_POINT('Ctrl Pts',(-59.58325,-3.64266772742874,-3.443299223485));
#33284=CARTESIAN_POINT('Ctrl Pts',(-59.58325,-3.71158231514896,-3.38072490033225));
#33285=CARTESIAN_POINT('Ctrl Pts',(-59.58325,-3.74837014811767,-3.34732161338785));
#33286=CARTESIAN_POINT('Ctrl Pts',(-59.58325,-3.78467562111936,-3.31335974384355));
#33287=CARTESIAN_POINT('Ctrl Pts',(-59.58325,-3.82048860435084,-3.27885213139493));
#33288=CARTESIAN_POINT('Ctrl Pts',(-59.58325,-3.84234667310303,-3.25779078164642));
#33289=CARTESIAN_POINT('Ctrl Pts',(-59.58325,-3.86402127513146,-3.23652612382414));
#33290=CARTESIAN_POINT('Ctrl Pts',(-59.58325,-3.8855100329079,-3.21506097592997));
#33291=CARTESIAN_POINT('Ctrl Pts',(-59.58325,-3.90210456603726,-3.19848467535634));
#33292=CARTESIAN_POINT('Ctrl Pts',(-59.58325,-3.91858452173466,-3.18179249883958));
#33293=CARTESIAN_POINT('Ctrl Pts',(-59.58325,-3.93494336450657,-3.16499175093224));
#33294=CARTESIAN_POINT('Ctrl Pts',(-59.58325,-4.03888838843746,-3.05823883646053));
#33295=CARTESIAN_POINT('Ctrl Pts',(-59.58325,-4.1380152907603,-2.94703675275575));
#33296=CARTESIAN_POINT('Ctrl Pts',(-59.58325,-4.23209117418264,-2.83177988663891));
#33297=CARTESIAN_POINT('Ctrl Pts',(-59.58325,-4.32673851465113,-2.71582290115179));
#33298=CARTESIAN_POINT('Ctrl Pts',(-59.58325,-4.41627390021231,-2.59576123435737));
#33299=CARTESIAN_POINT('Ctrl Pts',(-59.58325,-4.50043285477973,-2.47195122881639));
#33300=CARTESIAN_POINT('Ctrl Pts',(-59.58325,-4.55927868770607,-2.38538048969394));
#33301=CARTESIAN_POINT('Ctrl Pts',(-59.58325,-4.61549536035516,-2.29697618702752));
#33302=CARTESIAN_POINT('Ctrl Pts',(-59.58325,-4.66898213393302,-2.20684909182908));
#33303=CARTESIAN_POINT('Ctrl Pts',(-59.58325,-4.68018502488076,-2.18797182645289));
#33304=CARTESIAN_POINT('Ctrl Pts',(-59.58325,-4.6912681217303,-2.16901895381225));
#33305=CARTESIAN_POINT('Ctrl Pts',(-59.58325,-4.70223044399627,-2.14999144802621));
#33306=CARTESIAN_POINT('Ctrl Pts',(-59.58325,-4.71373786468606,-2.13001780481038));
#33307=CARTESIAN_POINT('Ctrl Pts',(-59.58325,-4.72510830074832,-2.10996863045952));
#33308=CARTESIAN_POINT('Ctrl Pts',(-59.58325,-4.73633763714775,-2.08985117085674));
#33309=CARTESIAN_POINT('Ctrl Pts',(-59.58325,-4.76548431241845,-2.03763463361387));
#33310=CARTESIAN_POINT('Ctrl Pts',(-59.58325,-4.79368754177112,-1.98494582209745));
#33311=CARTESIAN_POINT('Ctrl Pts',(-59.58325,-4.82093354346874,-1.93180915190821));
#33312=CARTESIAN_POINT('Ctrl Pts',(-59.58325,-4.88897898047618,-1.79910315033508));
#33313=CARTESIAN_POINT('Ctrl Pts',(-59.58325,-4.95105661819981,-1.66360652146873));
#33314=CARTESIAN_POINT('Ctrl Pts',(-59.58325,-5.00718259483252,-1.52577115922053));
#33315=CARTESIAN_POINT('Ctrl Pts',(-59.58325,-5.06418821702403,-1.38577554477676));
#33316=CARTESIAN_POINT('Ctrl Pts',(-59.58325,-5.11505449397166,-1.24336673915174));
#33317=CARTESIAN_POINT('Ctrl Pts',(-59.58325,-5.15975833801014,-1.09898206153507));
#33318=CARTESIAN_POINT('Ctrl Pts',(-59.58325,-5.20488323012226,-0.953237480946295));
#33319=CARTESIAN_POINT('Ctrl Pts',(-59.58325,-5.24372938483295,-0.805478959672225));
#33320=CARTESIAN_POINT('Ctrl Pts',(-59.58325,-5.27622766283853,-0.656129274418985));
#33321=CARTESIAN_POINT('Ctrl Pts',(-59.58325,-5.29940736442347,-0.549604210679269));
#33322=CARTESIAN_POINT('Ctrl Pts',(-59.58325,-5.3193567154633,-0.442269066215297));
#33323=CARTESIAN_POINT('Ctrl Pts',(-59.58325,-5.33603533027086,-0.334271925679514));
#33324=CARTESIAN_POINT('Ctrl Pts',(-59.58325,-5.34099072117784,-0.302184845645285));
#33325=CARTESIAN_POINT('Ctrl Pts',(-59.58325,-5.34565730024493,-0.27003930767804));
#33326=CARTESIAN_POINT('Ctrl Pts',(-59.58325,-5.35003377981377,-0.237839152221993));
#33327=CARTESIAN_POINT('Ctrl Pts',(-59.58325,-5.352660372538,-0.218513872003155));
#33328=CARTESIAN_POINT('Ctrl Pts',(-59.58325,-5.35518231401894,-0.199169720534567));
#33329=CARTESIAN_POINT('Ctrl Pts',(-59.58325,-5.35759784303445,-0.17982062955677));
#33330=CARTESIAN_POINT('Ctrl Pts',(-59.58325,-5.37701026531633,-0.024321472883059));
#33331=CARTESIAN_POINT('Ctrl Pts',(-59.58325,-5.38958429037093,0.13171511776847));
#33332=CARTESIAN_POINT('Ctrl Pts',(-59.58325,-5.3953137326205,0.287821200437283));
#33333=CARTESIAN_POINT('Ctrl Pts',(-59.58325,-5.39967792196466,0.40672919756276));
#33334=CARTESIAN_POINT('Ctrl Pts',(-59.58325,-5.40006999862904,0.525678303322171));
#33335=CARTESIAN_POINT('Ctrl Pts',(-59.58325,-5.39646930124031,0.644471130262479));
#33336=CARTESIAN_POINT('Ctrl Pts',(-59.58325,-5.39177018485815,0.799502575255909));
#33337=CARTESIAN_POINT('Ctrl Pts',(-59.58325,-5.38027275281682,0.954267914689577));
#33338=CARTESIAN_POINT('Ctrl Pts',(-59.58325,-5.36216621021034,1.10837045744723));
#33339=CARTESIAN_POINT('Ctrl Pts',(-59.58325,-5.34390859252952,1.26375878146143));
#33340=CARTESIAN_POINT('Ctrl Pts',(-59.58325,-5.31893107268399,1.41847392843383));
#33341=CARTESIAN_POINT('Ctrl Pts',(-59.58325,-5.28737476637574,1.57211259015712));
#33342=CARTESIAN_POINT('Ctrl Pts',(-59.58325,-5.27183516770569,1.64777046722494));
#33343=CARTESIAN_POINT('Ctrl Pts',(-59.58325,-5.2546994281243,1.7231672826984));
#33344=CARTESIAN_POINT('Ctrl Pts',(-59.58325,-5.23597979923346,1.79825433423466));
#33345=CARTESIAN_POINT('Ctrl Pts',(-59.58325,-5.22958197362955,1.82391690819068));
#33346=CARTESIAN_POINT('Ctrl Pts',(-59.58325,-5.222999112305,1.8495432939777));
#33347=CARTESIAN_POINT('Ctrl Pts',(-59.58325,-5.21623162451923,1.87513152788836));
#33348=CARTESIAN_POINT('Ctrl Pts',(-59.58325,-5.21116093774669,1.89430406625579));
#33349=CARTESIAN_POINT('Ctrl Pts',(-59.58325,-5.20598907532358,1.91344580701779));
#33350=CARTESIAN_POINT('Ctrl Pts',(-59.58325,-5.20071683417188,1.93255481558272));
#33351=CARTESIAN_POINT('Ctrl Pts',(-59.58325,-5.15824206256221,2.08650277644576));
#33352=CARTESIAN_POINT('Ctrl Pts',(-59.58325,-5.10925020939434,2.23834978988568));
#33353=CARTESIAN_POINT('Ctrl Pts',(-59.58325,-5.05397150557403,2.3876831941389));
#33354=CARTESIAN_POINT('Ctrl Pts',(-59.58325,-4.99583927336141,2.5447253013737));
#33355=CARTESIAN_POINT('Ctrl Pts',(-59.58325,-4.93075469787697,2.69898843399027));
#33356=CARTESIAN_POINT('Ctrl Pts',(-59.58325,-4.85892433062117,2.84999610861345));
#33357=CARTESIAN_POINT('Ctrl Pts',(-59.58325,-4.78709396336536,3.00100378323664));
#33358=CARTESIAN_POINT('Ctrl Pts',(-59.58325,-4.70851762016637,3.14875695019248));
#33359=CARTESIAN_POINT('Ctrl Pts',(-59.58325,-4.62334187522332,3.2927687170727));
#33360=CARTESIAN_POINT('Ctrl Pts',(-59.58325,-4.56177409370411,3.39686507696254));
#33361=CARTESIAN_POINT('Ctrl Pts',(-59.58325,-4.49675694033257,3.49900642576255));
#33362=CARTESIAN_POINT('Ctrl Pts',(-59.58325,-4.42842615286909,3.59907504329026));
#33363=CARTESIAN_POINT('Ctrl Pts',(-59.58325,-4.39835351315343,3.64311562285131));
#33364=CARTESIAN_POINT('Ctrl Pts',(-59.58325,-4.36763885459402,3.68675462947469));
#33365=CARTESIAN_POINT('Ctrl Pts',(-59.58325,-4.33629285797398,3.72998149499838));
#33366=CARTESIAN_POINT('Ctrl Pts',(-59.58325,-4.3166147172816,3.75711811316934));
#33367=CARTESIAN_POINT('Ctrl Pts',(-59.58325,-4.2966877571498,3.78409230058656));
#33368=CARTESIAN_POINT('Ctrl Pts',(-59.58325,-4.27651451736783,3.81090136797568));
#33369=CARTESIAN_POINT('Ctrl Pts',(-59.58325,-4.26373058384259,3.82789047528221));
#33370=CARTESIAN_POINT('Ctrl Pts',(-59.58325,-4.25084725050488,3.84481382990744));
#33371=CARTESIAN_POINT('Ctrl Pts',(-59.58325,-4.23787521996861,3.86165791344566));
#33372=CARTESIAN_POINT('Ctrl Pts',(-59.58325,-4.13930729891155,3.98964761342608));
#33373=CARTESIAN_POINT('Ctrl Pts',(-59.58325,-4.03548977851738,4.11323945679425));
#33374=CARTESIAN_POINT('Ctrl Pts',(-59.58325,-3.92682461937095,4.23220103909675));
#33375=CARTESIAN_POINT('Ctrl Pts',(-59.58325,-3.81589473640299,4.35364193612537));
#33376=CARTESIAN_POINT('Ctrl Pts',(-59.58325,-3.69991275233022,4.47025816964232));
#33377=CARTESIAN_POINT('Ctrl Pts',(-59.58325,-3.57925525293198,4.58178425450939));
#33378=CARTESIAN_POINT('Ctrl Pts',(-59.58325,-3.45813211677665,4.69374073653162));
#33379=CARTESIAN_POINT('Ctrl Pts',(-59.58325,-3.33229684896289,4.80056830700697));
#33380=CARTESIAN_POINT('Ctrl Pts',(-59.58325,-3.20208544403337,4.9019710938485));
#33381=CARTESIAN_POINT('Ctrl Pts',(-59.58325,-3.07288444991452,5.00258701818661));
#33382=CARTESIAN_POINT('Ctrl Pts',(-59.58325,-2.9393744417493,5.09786256374746));
#33383=CARTESIAN_POINT('Ctrl Pts',(-59.58325,-2.80184697473418,5.18747342871888));
#33384=CARTESIAN_POINT('Ctrl Pts',(-59.58325,-2.730280444168,5.2341051223451));
#33385=CARTESIAN_POINT('Ctrl Pts',(-59.58325,-2.65762544766573,5.27920221586187));
#33386=CARTESIAN_POINT('Ctrl Pts',(-59.58325,-2.58391981634397,5.32271443393359));
#33387=CARTESIAN_POINT('Ctrl Pts',(-59.58325,-2.85728527160914,-4.0034352877952));
#33388=CARTESIAN_POINT('Ctrl Pts',(-59.5433136744572,-2.28297233951893,
-4.4125035738704));
#33389=CARTESIAN_POINT('Ctrl Pts',(-59.4569578008868,-0.848960315252899,
-5.02880402090236));
#33390=CARTESIAN_POINT('Ctrl Pts',(-59.3241823792888,1.56581406446455,-4.88302020893749));
#33391=CARTESIAN_POINT('Ctrl Pts',(-59.184923735206,3.71514791027481,-3.53457280157081));
#33392=CARTESIAN_POINT('Ctrl Pts',(-59.0456650911232,4.95490602150955,-1.32078475768876));
#33393=CARTESIAN_POINT('Ctrl Pts',(-58.9064064470403,4.98156463212109,1.21638024324112));
#33394=CARTESIAN_POINT('Ctrl Pts',(-58.7671478029575,3.78859490309226,3.45573509562084));
#33395=CARTESIAN_POINT('Ctrl Pts',(-58.6278891588746,1.66807055469799,4.84903148731836));
#33396=CARTESIAN_POINT('Ctrl Pts',(-58.4886305147918,-0.860844735280108,
5.05514653385482));
#33397=CARTESIAN_POINT('Ctrl Pts',(-58.349371870709,-3.17900084006467,4.02361981064615));
#33398=CARTESIAN_POINT('Ctrl Pts',(-58.2191981777753,-4.61839135830064,
2.13855734824838));
#33399=CARTESIAN_POINT('Ctrl Pts',(-58.1354440328692,-4.91765907220889,
0.659097939802908));
#33400=CARTESIAN_POINT('Ctrl Pts',(-58.0981094359908,-4.91834149996792,
-0.000124244451390268));
#33401=CARTESIAN_POINT('Origin',(-59.58325,-7.01450167938425E-16,0.));
#33402=CARTESIAN_POINT('',(-59.58325,-5.91675,-7.2459289488551E-16));
#33403=CARTESIAN_POINT('Origin',(-59.58325,0.,0.));
#33404=CARTESIAN_POINT('Origin',(-59.58325,0.,0.));
#33405=CARTESIAN_POINT('',(-59.58325,2.8570646345847,-4.0032942355397));
#33406=CARTESIAN_POINT('Ctrl Pts',(-59.58325,2.58415317085794,5.32292607787884));
#33407=CARTESIAN_POINT('Ctrl Pts',(-59.58325,2.70296646487954,5.25292992541471));
#33408=CARTESIAN_POINT('Ctrl Pts',(-59.58325,2.81915569555313,5.17883110287497));
#33409=CARTESIAN_POINT('Ctrl Pts',(-59.58325,2.93247861654453,5.10069749527868));
#33410=CARTESIAN_POINT('Ctrl Pts',(-59.58325,3.06920329489612,5.00642890183267));
#33411=CARTESIAN_POINT('Ctrl Pts',(-59.58325,3.20175694045079,4.90628756576197));
#33412=CARTESIAN_POINT('Ctrl Pts',(-59.58325,3.32982749537687,4.80061426652425));
#33413=CARTESIAN_POINT('Ctrl Pts',(-59.58325,3.45739810776431,4.69535347879252));
#33414=CARTESIAN_POINT('Ctrl Pts',(-59.58325,3.58052099337265,4.58460318693842));
#33415=CARTESIAN_POINT('Ctrl Pts',(-59.58325,3.69884497680949,4.46867157675984));
#33416=CARTESIAN_POINT('Ctrl Pts',(-59.58325,3.72630240576341,4.44176930506873));
#33417=CARTESIAN_POINT('Ctrl Pts',(-59.58325,3.75350122285113,4.41458792820906));
#33418=CARTESIAN_POINT('Ctrl Pts',(-59.58325,3.78043667074496,4.38713113248787));
#33419=CARTESIAN_POINT('Ctrl Pts',(-59.58325,3.79756513892093,4.36967113503105));
#33420=CARTESIAN_POINT('Ctrl Pts',(-59.58325,3.81458599818276,4.35210081720947));
#33421=CARTESIAN_POINT('Ctrl Pts',(-59.58325,3.83148983927773,4.33442994372371));
#33422=CARTESIAN_POINT('Ctrl Pts',(-59.58325,3.94443075290801,4.2163641984937));
#33423=CARTESIAN_POINT('Ctrl Pts',(-59.58325,4.05225471233772,4.09370721020746));
#33424=CARTESIAN_POINT('Ctrl Pts',(-59.58325,4.15466130575339,3.96678643366706));
#33425=CARTESIAN_POINT('Ctrl Pts',(-59.58325,4.2563159827758,3.84079756794747));
#33426=CARTESIAN_POINT('Ctrl Pts',(-59.58325,4.35263292305005,3.7106066599572));
#33427=CARTESIAN_POINT('Ctrl Pts',(-59.58325,4.44327305063394,3.57651053181448));
#33428=CARTESIAN_POINT('Ctrl Pts',(-59.58325,4.5116269274949,3.47538545095982));
#33429=CARTESIAN_POINT('Ctrl Pts',(-59.58325,4.57675150588568,3.37203892619259));
#33430=CARTESIAN_POINT('Ctrl Pts',(-59.58325,4.63848222257101,3.26659257919084));
#33431=CARTESIAN_POINT('Ctrl Pts',(-59.58325,4.65762303654452,3.23389688050918));
#33432=CARTESIAN_POINT('Ctrl Pts',(-59.58325,4.67643742778736,3.20099927304137));
#33433=CARTESIAN_POINT('Ctrl Pts',(-59.58325,4.6949201424431,3.16790332449171));
#33434=CARTESIAN_POINT('Ctrl Pts',(-59.58325,4.7055680211765,3.14883677213252));
#33435=CARTESIAN_POINT('Ctrl Pts',(-59.58325,4.71610083541303,3.12971330580686));
#33436=CARTESIAN_POINT('Ctrl Pts',(-59.58325,4.72651757868068,3.1105343324428));
#33437=CARTESIAN_POINT('Ctrl Pts',(-59.58325,4.75633369194143,3.05563786169807));
#33438=CARTESIAN_POINT('Ctrl Pts',(-59.58325,4.7851998467299,3.00028502027509));
#33439=CARTESIAN_POINT('Ctrl Pts',(-59.58325,4.81309966376949,2.94449416952489));
#33440=CARTESIAN_POINT('Ctrl Pts',(-59.58325,4.88433135386074,2.80205321426967));
#33441=CARTESIAN_POINT('Ctrl Pts',(-59.58325,4.94926756855005,2.65675835282064));
#33442=CARTESIAN_POINT('Ctrl Pts',(-59.58325,5.00784297450621,2.5090468261143));
#33443=CARTESIAN_POINT('Ctrl Pts',(-59.58325,5.0666367561758,2.36078461419289));
#33444=CARTESIAN_POINT('Ctrl Pts',(-59.58325,5.1190223304161,2.21008689945141));
#33445=CARTESIAN_POINT('Ctrl Pts',(-59.58325,5.16488256999809,2.05738435244192));
#33446=CARTESIAN_POINT('Ctrl Pts',(-59.58325,5.21012932720205,1.90672454054514));
#33447=CARTESIAN_POINT('Ctrl Pts',(-59.58325,5.24902413845654,1.75411243330923));
#33448=CARTESIAN_POINT('Ctrl Pts',(-59.58325,5.28140444330562,1.59996188041636));
#33449=CARTESIAN_POINT('Ctrl Pts',(-59.58325,5.30441106192448,1.49043595109536));
#33450=CARTESIAN_POINT('Ctrl Pts',(-59.58325,5.32412794044939,1.38013335563645));
#33451=CARTESIAN_POINT('Ctrl Pts',(-59.58325,5.34048114038691,1.26920566262887));
#33452=CARTESIAN_POINT('Ctrl Pts',(-59.58325,5.34621139891097,1.23033593922064));
#33453=CARTESIAN_POINT('Ctrl Pts',(-59.58325,5.35152853242856,1.19138949828347));
#33454=CARTESIAN_POINT('Ctrl Pts',(-59.58325,5.35642897582421,1.152372989026));
#33455=CARTESIAN_POINT('Ctrl Pts',(-59.58325,5.359318940468,1.12936357473948));
#33456=CARTESIAN_POINT('Ctrl Pts',(-59.58325,5.36206407119635,1.106328380616));
#33457=CARTESIAN_POINT('Ctrl Pts',(-59.58325,5.36466150365874,1.08328926655645));
#33458=CARTESIAN_POINT('Ctrl Pts',(-59.58325,5.3820688210545,0.928887111058601));
#33459=CARTESIAN_POINT('Ctrl Pts',(-59.58325,5.39287439304195,0.774098737382789));
#33460=CARTESIAN_POINT('Ctrl Pts',(-59.58325,5.39698732754428,0.619324715726741));
#33461=CARTESIAN_POINT('Ctrl Pts',(-59.58325,5.40012959795112,0.501077797931173));
#33462=CARTESIAN_POINT('Ctrl Pts',(-59.58325,5.39936439889502,0.382839033567496));
#33463=CARTESIAN_POINT('Ctrl Pts',(-59.58325,5.39463071560031,0.264788458795355));
#33464=CARTESIAN_POINT('Ctrl Pts',(-59.58325,5.38840882171842,0.109624265671113));
#33465=CARTESIAN_POINT('Ctrl Pts',(-59.58325,5.3753324281636,-0.0452158194266503));
#33466=CARTESIAN_POINT('Ctrl Pts',(-59.58325,5.35550293155849,-0.199293539444912));
#33467=CARTESIAN_POINT('Ctrl Pts',(-59.58325,5.33581130130685,-0.352300020296972));
#33468=CARTESIAN_POINT('Ctrl Pts',(-59.58325,5.30945980007245,-0.504555404036452));
#33469=CARTESIAN_POINT('Ctrl Pts',(-59.58325,5.27650250311296,-0.655606684917678));
#33470=CARTESIAN_POINT('Ctrl Pts',(-59.58325,5.26118504007137,-0.725810331021533));
#33471=CARTESIAN_POINT('Ctrl Pts',(-59.58325,5.24444006104799,-0.795753478288869));
#33472=CARTESIAN_POINT('Ctrl Pts',(-59.58325,5.22626994654444,-0.865388232001238));
#33473=CARTESIAN_POINT('Ctrl Pts',(-59.58325,5.22064316880509,-0.886952173273992));
#33474=CARTESIAN_POINT('Ctrl Pts',(-59.58325,5.21487971172168,-0.908486528003936));
#33475=CARTESIAN_POINT('Ctrl Pts',(-59.58325,5.20897961039385,-0.929989838884862));
#33476=CARTESIAN_POINT('Ctrl Pts',(-59.58325,5.20439703260389,-0.946691347787532));
#33477=CARTESIAN_POINT('Ctrl Pts',(-59.58325,5.19973235987882,-0.963372783691243));
#33478=CARTESIAN_POINT('Ctrl Pts',(-59.58325,5.1949883654161,-0.980024246908933));
#33479=CARTESIAN_POINT('Ctrl Pts',(-59.58325,5.15340085215999,-1.12599679235358));
#33480=CARTESIAN_POINT('Ctrl Pts',(-59.58325,5.10566795980971,-1.26986449671757));
#33481=CARTESIAN_POINT('Ctrl Pts',(-59.58325,5.05191863367101,-1.41122890907032));
#33482=CARTESIAN_POINT('Ctrl Pts',(-59.58325,4.99658445894275,-1.55676158185768));
#33483=CARTESIAN_POINT('Ctrl Pts',(-59.58325,4.93487370729753,-1.69964208005801));
#33484=CARTESIAN_POINT('Ctrl Pts',(-59.58325,4.86687602556661,-1.83940847048739));
#33485=CARTESIAN_POINT('Ctrl Pts',(-59.58325,4.79887834383569,-1.97917486091677));
#33486=CARTESIAN_POINT('Ctrl Pts',(-59.58325,4.72459337675515,-2.11582794888444));
#33487=CARTESIAN_POINT('Ctrl Pts',(-59.58325,4.64406438290419,-2.24886612391969));
#33488=CARTESIAN_POINT('Ctrl Pts',(-59.58325,4.589502138863,-2.33900584907884));
#33489=CARTESIAN_POINT('Ctrl Pts',(-59.58325,4.5320723280881,-2.42748516111421));
#33490=CARTESIAN_POINT('Ctrl Pts',(-59.58325,4.47186625223104,-2.51418020727366));
#33491=CARTESIAN_POINT('Ctrl Pts',(-59.58325,4.44033492565804,-2.55958442559882));
#33492=CARTESIAN_POINT('Ctrl Pts',(-59.58325,4.40804200014479,-2.6044990694282));
#33493=CARTESIAN_POINT('Ctrl Pts',(-59.58325,4.37499996200529,-2.64890512365198));
#33494=CARTESIAN_POINT('Ctrl Pts',(-59.58325,4.35433201309379,-2.67668131760779));
#33495=CARTESIAN_POINT('Ctrl Pts',(-59.58325,4.33337096128033,-2.70425850563629));
#33496=CARTESIAN_POINT('Ctrl Pts',(-59.58325,4.31211979047038,-2.73163185516577));
#33497=CARTESIAN_POINT('Ctrl Pts',(-59.58325,4.29993198098909,-2.74733080991578));
#33498=CARTESIAN_POINT('Ctrl Pts',(-59.58325,4.28765459229105,-2.76295516788741));
#33499=CARTESIAN_POINT('Ctrl Pts',(-59.58325,4.27529017002798,-2.77850208462221));
#33500=CARTESIAN_POINT('Ctrl Pts',(-59.58325,4.18361908532631,-2.89376850714675));
#33501=CARTESIAN_POINT('Ctrl Pts',(-59.58325,4.08713606344259,-3.00482084934681));
#33502=CARTESIAN_POINT('Ctrl Pts',(-59.58325,3.9861531884936,-3.11138603574584));
#33503=CARTESIAN_POINT('Ctrl Pts',(-59.58325,3.88521216477139,-3.21790705739133));
#33504=CARTESIAN_POINT('Ctrl Pts',(-59.58325,3.77977437828728,-3.31994511155099));
#33505=CARTESIAN_POINT('Ctrl Pts',(-59.58325,3.67011934868638,-3.41718718499577));
#33506=CARTESIAN_POINT('Ctrl Pts',(-59.58325,3.56151642211555,-3.51349625353879));
#33507=CARTESIAN_POINT('Ctrl Pts',(-59.58325,3.44877615893273,-3.60510130706221));
#33508=CARTESIAN_POINT('Ctrl Pts',(-59.58325,3.33214805491118,-3.69165255083082));
#33509=CARTESIAN_POINT('Ctrl Pts',(-59.58325,3.21805378133788,-3.77632340583177));
#33510=CARTESIAN_POINT('Ctrl Pts',(-59.58325,3.10023818545153,-3.85615788944432));
#33511=CARTESIAN_POINT('Ctrl Pts',(-59.58325,2.97892256809559,-3.93078028943487));
#33512=CARTESIAN_POINT('Ctrl Pts',(-59.58325,2.9386857006511,-3.95553037258368));
#33513=CARTESIAN_POINT('Ctrl Pts',(-59.58325,2.89806374610355,-3.97970668204472));
#33514=CARTESIAN_POINT('Ctrl Pts',(-59.58325,2.85706463458446,-4.00329423553987));
#33515=CARTESIAN_POINT('Origin',(-59.58325,0.,0.));
#33516=CARTESIAN_POINT('Origin',(-62.8183905640093,0.,0.));
#33517=CARTESIAN_POINT('Ctrl Pts',(-59.58325,2.85706463458446,-4.00329423553987));
#33518=CARTESIAN_POINT('Ctrl Pts',(-59.5368304519724,3.52427108824591,-3.52712339958193));
#33519=CARTESIAN_POINT('Ctrl Pts',(-59.4439913559172,4.61530848209962,-2.23520568907806));
#33520=CARTESIAN_POINT('Ctrl Pts',(-59.3047327118343,5.12174738739822,0.251511598513074));
#33521=CARTESIAN_POINT('Ctrl Pts',(-59.1654740677515,4.3742789497841,2.67597888304926));
#33522=CARTESIAN_POINT('Ctrl Pts',(-59.0262154236687,2.55584624568566,4.44562215581043));
#33523=CARTESIAN_POINT('Ctrl Pts',(-58.8869567795858,0.111678748687467,
5.12668320818063));
#33524=CARTESIAN_POINT('Ctrl Pts',(-58.747698135503,-2.35983518894881,4.55267369514457));
#33525=CARTESIAN_POINT('Ctrl Pts',(-58.60843949142,-4.25359264236838,2.86399697899764));
#33526=CARTESIAN_POINT('Ctrl Pts',(-58.5070036342556,-4.87445011480876,
1.12323890322437));
#33527=CARTESIAN_POINT('Ctrl Pts',(-58.4519873251187,-4.91852463110708,
0.151914236828057));
#33528=CARTESIAN_POINT('Ctrl Pts',(-58.4433905640093,-4.91836886135133,
0.000122455552848399));
#33529=CARTESIAN_POINT('Ctrl Pts',(-60.1597342437858,3.43710408716083,-4.81604049573115));
#33530=CARTESIAN_POINT('Ctrl Pts',(-60.1133146957582,4.23976637246581,-4.24319775824234));
#33531=CARTESIAN_POINT('Ctrl Pts',(-60.020475599703,5.55230548700525,-2.68899573239491));
#33532=CARTESIAN_POINT('Ctrl Pts',(-59.8812169556201,6.16156129810163,0.302573323947274));
#33533=CARTESIAN_POINT('Ctrl Pts',(-59.7419583115374,5.2623422916961,3.21925442104062));
#33534=CARTESIAN_POINT('Ctrl Pts',(-59.6026996674544,3.07473253172559,5.34816955022458));
#33535=CARTESIAN_POINT('Ctrl Pts',(-59.4634410233717,0.134351697513361,
6.16749918609318));
#33536=CARTESIAN_POINT('Ctrl Pts',(-59.3241823792887,-2.83892743439519,
5.47695462527239));
#33537=CARTESIAN_POINT('Ctrl Pts',(-59.184923735206,-5.11715432658648,3.44544383174565));
#33538=CARTESIAN_POINT('Ctrl Pts',(-59.0456650911231,-6.14255875840504,
0.570418363169113));
#33539=CARTESIAN_POINT('Ctrl Pts',(-58.9064064470402,-5.66409071331427,
-2.44427558051098));
#33540=CARTESIAN_POINT('Ctrl Pts',(-58.7671478029575,-3.79889373407555,
-4.86053471086364));
#33541=CARTESIAN_POINT('Ctrl Pts',(-58.6278891588746,-1.0036201493159,-6.08680140714466));
#33542=CARTESIAN_POINT('Ctrl Pts',(-58.4886305147919,2.03736788399004,-5.82284542089895));
#33543=CARTESIAN_POINT('Ctrl Pts',(-58.3493718707089,4.57955079663083,-4.13329347110169));
#33544=CARTESIAN_POINT('Ctrl Pts',(-58.2101132266262,6.00053037756086,-1.43179411094106));
#33545=CARTESIAN_POINT('Ctrl Pts',(-58.0708545825432,5.95241075130211,1.62024861133869));
#33546=CARTESIAN_POINT('Ctrl Pts',(-57.9315959384605,4.44697294148773,4.27560886674674));
#33547=CARTESIAN_POINT('Ctrl Pts',(-57.7923372943776,1.85279062942082,5.88417931287061));
#33548=CARTESIAN_POINT('Ctrl Pts',(-57.6530786502948,-1.19500713116077,
6.05213659818529));
#33549=CARTESIAN_POINT('Ctrl Pts',(-57.5138200062119,-3.95023341240051,
4.73835998660194));
#33550=CARTESIAN_POINT('Ctrl Pts',(-57.3745613621291,-5.73833104722617,
2.26449910444055));
#33551=CARTESIAN_POINT('Ctrl Pts',(-57.2353027180462,-6.12152325938902,
-0.763775085538537));
#33552=CARTESIAN_POINT('Ctrl Pts',(-57.0960440739634,-5.00599377891902,
-3.60505557232192));
#33553=CARTESIAN_POINT('Ctrl Pts',(-56.9567854298806,-2.66485571171295,
-5.56371669240644));
#33554=CARTESIAN_POINT('Ctrl Pts',(-56.8175267857977,0.328714257451459,
-6.1602229125286));
#33555=CARTESIAN_POINT('Ctrl Pts',(-56.6782681417149,3.24180569743506,-5.24853267271102));
#33556=CARTESIAN_POINT('Ctrl Pts',(-56.5390094976321,5.36121159272567,-3.05185347844784));
#33557=CARTESIAN_POINT('Ctrl Pts',(-56.3997508535491,6.16804155340788,-0.10799440477762));
#33558=CARTESIAN_POINT('Ctrl Pts',(-56.2604922094665,5.46476082983919,2.86230474769956));
#33559=CARTESIAN_POINT('Ctrl Pts',(-56.1212335653834,3.42355239541739,5.13183090054873));
#33560=CARTESIAN_POINT('Ctrl Pts',(-55.9819749213008,0.544161694283669,
6.14493998721812));
#33561=CARTESIAN_POINT('Ctrl Pts',(-55.8427162772178,-2.46845515025061,
5.6535943051491));
#33562=CARTESIAN_POINT('Ctrl Pts',(-55.7034576331351,-4.87672449425258,
3.77808914706642));
#33563=CARTESIAN_POINT('Ctrl Pts',(-55.5641989890521,-6.091034021489,0.977601117575148));
#33564=CARTESIAN_POINT('Ctrl Pts',(-55.4249403449694,-5.81408648206527,
-2.06223126130096));
#33565=CARTESIAN_POINT('Ctrl Pts',(-55.2856817008865,-4.11368645132967,
-4.59717121458057));
#33566=CARTESIAN_POINT('Ctrl Pts',(-55.1464230568037,-1.40613985583562,
-6.00659388521078));
#33567=CARTESIAN_POINT('Ctrl Pts',(-55.0071644127209,1.6456694689963,-5.94543281812475));
#33568=CARTESIAN_POINT('Ctrl Pts',(-54.867905768638,4.29457245372739,-4.42866196900453));
#33569=CARTESIAN_POINT('Ctrl Pts',(-54.7286471245552,5.89204287424835,-1.82762965724471));
#33570=CARTESIAN_POINT('Ctrl Pts',(-54.5893884804723,6.04697487809177,1.22085798508602));
#33571=CARTESIAN_POINT('Ctrl Pts',(-54.4501298363896,4.72143673728365,3.97044513019));
#33572=CARTESIAN_POINT('Ctrl Pts',(-54.3108711923066,2.23995760609141,5.74795522937805));
#33573=CARTESIAN_POINT('Ctrl Pts',(-54.1716125482238,-0.789926376776022,
6.11820363467045));
#33574=CARTESIAN_POINT('Ctrl Pts',(-54.032353904141,-3.62641408450318,4.99054308504978));
#33575=CARTESIAN_POINT('Ctrl Pts',(-53.8930952600581,-5.57505325763465,
2.64105671475614));
#33576=CARTESIAN_POINT('Ctrl Pts',(-53.7538366159754,-6.15876202024408,
-0.355034891271801));
#33577=CARTESIAN_POINT('Ctrl Pts',(-53.6145779718924,-5.23463199026661,
-3.26420393396288));
#33578=CARTESIAN_POINT('Ctrl Pts',(-53.4753193278097,-3.02891628545778,
-5.37420371140784));
#33579=CARTESIAN_POINT('Ctrl Pts',(-53.3360606837268,-0.0816363734756486,
-6.16844671684429));
#33580=CARTESIAN_POINT('Ctrl Pts',(-53.1968020396439,2.88563042717145,-5.4524798425857));
#33581=CARTESIAN_POINT('Ctrl Pts',(-53.0575433955611,5.14641344343852,-3.40159198982133));
#33582=CARTESIAN_POINT('Ctrl Pts',(-52.9182847514783,6.14720917537799,-0.517898397535566));
#33583=CARTESIAN_POINT('Ctrl Pts',(-52.7790261073954,5.64299457726843,2.49259134174462));
#33584=CARTESIAN_POINT('Ctrl Pts',(-52.6397674633126,3.75721561573744,4.89282435949625));
#33585=CARTESIAN_POINT('Ctrl Pts',(-52.5005088192298,0.951564212488417,
6.09515585900251));
#33586=CARTESIAN_POINT('Ctrl Pts',(-52.361250175147,-2.08705697080914,5.80522114967365));
#33587=CARTESIAN_POINT('Ctrl Pts',(-52.2219915310641,-4.61470769404007,
4.09400443265376));
#33588=CARTESIAN_POINT('Ctrl Pts',(-52.0827328869813,-6.01254770942893,
1.38045986463286));
#33589=CARTESIAN_POINT('Ctrl Pts',(-51.9434742428984,-5.93834632286783,
-1.67106024598258));
#33590=CARTESIAN_POINT('Ctrl Pts',(-51.8042155988156,-4.41027012834964,
-4.31345763755807));
#33591=CARTESIAN_POINT('Ctrl Pts',(-51.6649569547327,-1.8024353129505,-5.8997988388292));
#33592=CARTESIAN_POINT('Ctrl Pts',(-51.5256983106499,1.24668654634832,-6.04170274435736));
#33593=CARTESIAN_POINT('Ctrl Pts',(-51.3864396665671,3.99058434753268,-4.70442727239442));
#33594=CARTESIAN_POINT('Ctrl Pts',(-51.2471810224842,5.75747445390417,-2.21537520719677));
#33595=CARTESIAN_POINT('Ctrl Pts',(-51.1079223784014,6.11477229150658,0.81606324451273));
#33596=CARTESIAN_POINT('Ctrl Pts',(-50.9686637343185,4.97500126386264,3.6477063780664));
#33597=CARTESIAN_POINT('Ctrl Pts',(-50.8294050902357,2.61720949208814,5.58628802251951));
#33598=CARTESIAN_POINT('Ctrl Pts',(-50.6901464461529,-0.381349042150201,
6.15718866887091));
#33599=CARTESIAN_POINT('Ctrl Pts',(-50.55088780207,-3.28654256611867,5.22063572346428));
#33600=CARTESIAN_POINT('Ctrl Pts',(-50.4116291579872,-5.3870976971126,3.00592378442723));
#33601=CARTESIAN_POINT('Ctrl Pts',(-50.2723705139044,-6.168739244425,0.0552768515033475));
#33602=CARTESIAN_POINT('Ctrl Pts',(-50.1331118698215,-5.44009929303315,
-2.90890341502798));
#33603=CARTESIAN_POINT('Ctrl Pts',(-49.9938532257387,-3.37956947114509,
-5.16090201280022));
#33604=CARTESIAN_POINT('Ctrl Pts',(-49.8545945816558,-0.491625643961048,
-6.14936611548061));
#33605=CARTESIAN_POINT('Ctrl Pts',(-49.715335937573,2.51668201851298,-5.63229180828859));
#33606=CARTESIAN_POINT('Ctrl Pts',(-49.5760772934902,4.90883488175199,-3.73627347764));
#33607=CARTESIAN_POINT('Ctrl Pts',(-49.4368186494074,6.0991663989511,-0.925509931836011));
#33608=CARTESIAN_POINT('Ctrl Pts',(-49.2975600053245,5.79624981392584,2.11184457065046));
#33609=CARTESIAN_POINT('Ctrl Pts',(-49.1583013612417,4.07424765744423,4.63215990892277));
#33610=CARTESIAN_POINT('Ctrl Pts',(-49.0190427171588,1.35475466622873,6.01839174450722));
#33611=CARTESIAN_POINT('Ctrl Pts',(-48.879784073076,-1.69642050940358,5.93115139338866));
#33612=CARTESIAN_POINT('Ctrl Pts',(-48.7405254289932,-4.33226405763891,
4.39179775614853));
#33613=CARTESIAN_POINT('Ctrl Pts',(-48.6012667849103,-5.90744707306491,
1.77720805618193));
#33614=CARTESIAN_POINT('Ctrl Pts',(-48.4620081408274,-6.03632028911212,
-1.27249234311039));
#33615=CARTESIAN_POINT('Ctrl Pts',(-48.3227494967447,-4.68733190464862,
-4.01065069679278));
#33616=CARTESIAN_POINT('Ctrl Pts',(-48.1834908526618,-2.19075235554399,
-5.7668885469289));
#33617=CARTESIAN_POINT('Ctrl Pts',(-48.044232208579,0.842185210932005,-6.1112292925817));
#33618=CARTESIAN_POINT('Ctrl Pts',(-47.9049735644961,3.66893206449977,-4.95936859913705));
#33619=CARTESIAN_POINT('Ctrl Pts',(-47.7657149204133,5.59742078176774,-2.59331447916677));
#33620=CARTESIAN_POINT('Ctrl Pts',(-47.6264562763304,6.15550288721356,0.407656229593879));
#33621=CARTESIAN_POINT('Ctrl Pts',(-47.4871976322476,5.20654412783746,3.30882118599701));
#33622=CARTESIAN_POINT('Ctrl Pts',(-47.3479389881648,2.98287639521906,5.39989331439669));
#33623=CARTESIAN_POINT('Ctrl Pts',(-47.2086803440819,0.0289163201755667,
6.16891913080799));
#33624=CARTESIAN_POINT('Ctrl Pts',(-47.0694216999991,-2.93212328629913,
5.42761940725061));
#33625=CARTESIAN_POINT('Ctrl Pts',(-46.9301630559163,-5.17529634407517,
3.35748524151984));
#33626=CARTESIAN_POINT('Ctrl Pts',(-46.7909044118334,-6.1514107681389,0.465343913300744));
#33627=CARTESIAN_POINT('Ctrl Pts',(-46.6516457677506,-5.62148619364284,
-2.54072674065987));
#33628=CARTESIAN_POINT('Ctrl Pts',(-46.5123871236677,-3.71526311517727,
-4.92475576866757));
#33629=CARTESIAN_POINT('Ctrl Pts',(-46.3731284795849,-0.899438751369376,
-6.10306556810234));
#33630=CARTESIAN_POINT('Ctrl Pts',(-46.2338698355021,2.13659360820338,-5.78717263863846));
#33631=CARTESIAN_POINT('Ctrl Pts',(-46.0946111914193,4.6495275405512,-4.05441648645981));
#33632=CARTESIAN_POINT('Ctrl Pts',(-45.9553525473364,6.02412588373361,-1.32902473000016));
#33633=CARTESIAN_POINT('Ctrl Pts',(-45.8160939032536,5.92384816106664,1.72174979618084));
#33634=CARTESIAN_POINT('Ctrl Pts',(-45.6768352591706,4.37324518970676,4.35099137056464));
#33635=CARTESIAN_POINT('Ctrl Pts',(-45.537576615088,1.75194834758869,5.91498743729879));
#33636=CARTESIAN_POINT('Ctrl Pts',(-45.398317971005,-1.29827490415837,6.03082761063967));
#33637=CARTESIAN_POINT('Ctrl Pts',(-45.2590593269223,-4.03064381155875,
4.67015094620768));
#33638=CARTESIAN_POINT('Ctrl Pts',(-45.1198006828393,-5.77619733655087,
2.1660895007464));
#33639=CARTESIAN_POINT('Ctrl Pts',(-44.9805420387566,-6.10757470259099,
-0.868291799046749));
#33640=CARTESIAN_POINT('Ctrl Pts',(-44.8412833946737,-4.94364537632544,
-3.69009075622231));
#33641=CARTESIAN_POINT('Ctrl Pts',(-44.7020247505909,-2.56937211231493,
-5.60845133209513));
#33642=CARTESIAN_POINT('Ctrl Pts',(-44.562766106508,0.433955973233554,-6.15370470605441));
#33643=CARTESIAN_POINT('Ctrl Pts',(-44.4235074624252,3.33103938679021,-5.19235746069871));
#33644=CARTESIAN_POINT('Ctrl Pts',(-44.2842488183423,5.41259032961209,-2.95977453867871));
#33645=CARTESIAN_POINT('Ctrl Pts',(-44.1449901742595,6.16898637270852,-0.00255526083573153));
#33646=CARTESIAN_POINT('Ctrl Pts',(-44.0057315301767,5.41504041312089,2.95528961698998));
#33647=CARTESIAN_POINT('Ctrl Pts',(-43.8664728860938,3.33533970420366,5.18959617442281));
#33648=CARTESIAN_POINT('Ctrl Pts',(-43.727214242011,0.439053685459154,6.15334309601748));
#33649=CARTESIAN_POINT('Ctrl Pts',(-43.5879555979281,-2.56472506912859,
5.61057793064176));
#33650=CARTESIAN_POINT('Ctrl Pts',(-43.4486969538453,-4.94058672952753,
3.69418491199856));
#33651=CARTESIAN_POINT('Ctrl Pts',(-43.3094383097625,-6.10685329525738,
0.873351147148346));
#33652=CARTESIAN_POINT('Ctrl Pts',(-43.1701796656797,-5.77798978956076,
-2.16130363155039));
#33653=CARTESIAN_POINT('Ctrl Pts',(-43.0309210215968,-4.03451128181777,
-4.66681027179233));
#33654=CARTESIAN_POINT('Ctrl Pts',(-42.891662377514,-1.30327052577588,-6.02975002240266));
#33655=CARTESIAN_POINT('Ctrl Pts',(-42.7524037334311,1.74704764380147,-5.91643675925883));
#33656=CARTESIAN_POINT('Ctrl Pts',(-42.6131450893483,4.36963923437441,-4.35461276779428));
#33657=CARTESIAN_POINT('Ctrl Pts',(-42.4738864452654,5.92241979384368,-1.72665664841325));
#33658=CARTESIAN_POINT('Ctrl Pts',(-42.3346278011826,6.02522480923636,1.32403375870253));
#33659=CARTESIAN_POINT('Ctrl Pts',(-42.1953691570998,4.65288471079598,4.0505633267562));
#33660=CARTESIAN_POINT('Ctrl Pts',(-42.0561105130169,2.14138709314778,5.78540065279159));
#33661=CARTESIAN_POINT('Ctrl Pts',(-41.9168518689341,-0.89438253215062,
6.10380858826726));
#33662=CARTESIAN_POINT('Ctrl Pts',(-41.7775932248513,-3.71118206687627,
4.92783188253386));
#33663=CARTESIAN_POINT('Ctrl Pts',(-41.6383345807684,-5.61937947208383,
2.54538282872028));
#33664=CARTESIAN_POINT('Ctrl Pts',(-41.4990759366856,-6.15179415822822,
-0.460247792835837));
#33665=CARTESIAN_POINT('Ctrl Pts',(-41.3598172926027,-5.17807598109662,
-3.35319676279393));
#33666=CARTESIAN_POINT('Ctrl Pts',(-41.22055864852,-2.93661863664603,-5.42518851091134));
#33667=CARTESIAN_POINT('Ctrl Pts',(-41.081300004437,0.023805845163246,-6.16894096889873));
#33668=CARTESIAN_POINT('Ctrl Pts',(-40.9420413603543,2.97840198408325,-5.40236254033643));
#33669=CARTESIAN_POINT('Ctrl Pts',(-40.8027827162714,5.20380124272823,-3.31313326357414));
#33670=CARTESIAN_POINT('Ctrl Pts',(-40.6635240721886,6.15516306383205,-0.41275544049587));
#33671=CARTESIAN_POINT('Ctrl Pts',(-40.5242654281057,5.59956721847028,2.58867656570964));
#33672=CARTESIAN_POINT('Ctrl Pts',(-40.3850067840229,3.67303925299184,4.9563274752585));
#33673=CARTESIAN_POINT('Ctrl Pts',(-40.2457481399401,0.847247595532676,
6.11052951125231));
#33674=CARTESIAN_POINT('Ctrl Pts',(-40.1064894958572,-2.18597418948637,
5.76870143437157));
#33675=CARTESIAN_POINT('Ctrl Pts',(-39.9672308517744,-4.68400778706338,
4.01453240698724));
#33676=CARTESIAN_POINT('Ctrl Pts',(-39.8279722076915,-6.03526405781763,
1.27749252382781));
#33677=CARTESIAN_POINT('Ctrl Pts',(-39.6887135636088,-5.90891732329743,
-1.77231359032672));
#33678=CARTESIAN_POINT('Ctrl Pts',(-39.5494549195258,-4.33590083063914,
-4.38820730855825));
#33679=CARTESIAN_POINT('Ctrl Pts',(-39.4101962754431,-1.70133342048197,
-5.92974400698482));
#33680=CARTESIAN_POINT('Ctrl Pts',(-39.2709376313602,1.3497684363862,-6.01951198720932));
#33681=CARTESIAN_POINT('Ctrl Pts',(-39.1316789872773,4.07040887865475,-4.63553351369504));
#33682=CARTESIAN_POINT('Ctrl Pts',(-38.9924203431945,5.79449832759843,-2.11664558381422));
#33683=CARTESIAN_POINT('Ctrl Pts',(-38.8531616991117,6.09993101837978,0.92045693382662));
#33684=CARTESIAN_POINT('Ctrl Pts',(-38.7139030550289,4.91192840651688,3.73220561133409));
#33685=CARTESIAN_POINT('Ctrl Pts',(-38.574644410946,2.52134706642738,5.63020500218591));
#33686=CARTESIAN_POINT('Ctrl Pts',(-38.4353857668632,-0.486531208311943,
6.14977127862165));
#33687=CARTESIAN_POINT('Ctrl Pts',(-38.2961271227804,-3.37529290941433,
5.16369994981105));
#33688=CARTESIAN_POINT('Ctrl Pts',(-38.1568684786975,-5.43768762825154,
2.91340911194795));
#33689=CARTESIAN_POINT('Ctrl Pts',(-38.0176098346146,-6.16878292020774,
-0.0501665164674183));
#33690=CARTESIAN_POINT('Ctrl Pts',(-37.8783511905318,-5.38958602039518,
-3.00145996554709));
#33691=CARTESIAN_POINT('Ctrl Pts',(-37.739092546449,-3.29086632512096,-5.2179112896068));
#33692=CARTESIAN_POINT('Ctrl Pts',(-37.5998339023661,-0.386449658617007,
-6.15687063834997));
#33693=CARTESIAN_POINT('Ctrl Pts',(-37.4605752582833,2.61258079304851,-5.58845425818403));
#33694=CARTESIAN_POINT('Ctrl Pts',(-37.3213166142004,4.97197771843438,-3.65182652427703));
#33695=CARTESIAN_POINT('Ctrl Pts',(-37.1820579701176,6.11409414895942,-0.821128573173274));
#33696=CARTESIAN_POINT('Ctrl Pts',(-37.0427993260348,5.7593077426763,2.21060483152691));
#33697=CARTESIAN_POINT('Ctrl Pts',(-36.903540681952,3.99448022678247,4.70111977233776));
#33698=CARTESIAN_POINT('Ctrl Pts',(-36.7642820378691,1.25169119486223,6.04066788929217));
#33699=CARTESIAN_POINT('Ctrl Pts',(-36.6250233937863,-1.7975471744003,5.9012899904874));
#33700=CARTESIAN_POINT('Ctrl Pts',(-36.4857647497034,-4.40669525406299,
4.31710971992141));
#33701=CARTESIAN_POINT('Ctrl Pts',(-36.3465061056206,-5.93695994298196,
1.67597912619723));
#33702=CARTESIAN_POINT('Ctrl Pts',(-36.2072474615378,-6.01368924887476,
-1.37547846729399));
#33703=CARTESIAN_POINT('Ctrl Pts',(-36.0679888174549,-4.61809767173776,
-4.09018010487455));
#33704=CARTESIAN_POINT('Ctrl Pts',(-35.9287301733721,-2.09186542452573,
-5.80349019484784));
#33705=CARTESIAN_POINT('Ctrl Pts',(-35.7894715292893,0.946514527956128,
-6.09594206373299));
#33706=CARTESIAN_POINT('Ctrl Pts',(-35.6502128852064,3.75316100570587,-4.89593523867198));
#33707=CARTESIAN_POINT('Ctrl Pts',(-35.5109542411236,5.6409277247272,-2.49726526432922));
#33708=CARTESIAN_POINT('Ctrl Pts',(-35.3716955970407,6.14763610417245,0.512805739726707));
#33709=CARTESIAN_POINT('Ctrl Pts',(-35.2324369529579,5.14922962934839,3.39732742317573));
#33710=CARTESIAN_POINT('Ctrl Pts',(-35.093178308875,2.89014638839049,5.45008745339877));
#33711=CARTESIAN_POINT('Ctrl Pts',(-34.9539196647922,-0.0765262717307818,
6.16851222952148));
#33712=CARTESIAN_POINT('Ctrl Pts',(-34.8146610207094,-3.0244631403426,5.37671108659656));
#33713=CARTESIAN_POINT('Ctrl Pts',(-34.6754023766266,-5.23192605740906,
3.26853929543846));
#33714=CARTESIAN_POINT('Ctrl Pts',(-34.5361437325437,-6.15846578839096,
0.360136820166138));
#33715=CARTESIAN_POINT('Ctrl Pts',(-34.3968850884609,-5.57723925270567,
-2.63643731465406));
#33716=CARTESIAN_POINT('Ctrl Pts',(-34.2576264443781,-3.63054711319852,
-4.98753717328173));
#33717=CARTESIAN_POINT('Ctrl Pts',(-34.1183678002952,-0.794994557003578,
-6.1175471432884));
#33718=CARTESIAN_POINT('Ctrl Pts',(-33.9791091562124,2.23519510791631,-5.74980888600379));
#33719=CARTESIAN_POINT('Ctrl Pts',(-33.8398505121295,4.71814591515049,-3.97435510735641));
#33720=CARTESIAN_POINT('Ctrl Pts',(-33.7005918680467,6.04596141815232,-1.22586701001161));
#33721=CARTESIAN_POINT('Ctrl Pts',(-33.5613332239639,5.89355490010385,1.82274793525691));
#33722=CARTESIAN_POINT('Ctrl Pts',(-33.422074579881,4.29823977876676,4.42510273329878));
#33723=CARTESIAN_POINT('Ctrl Pts',(-33.2828159357982,1.6505942285284,5.94406747007215));
#33724=CARTESIAN_POINT('Ctrl Pts',(-33.1435572917153,-1.40116338196076,
6.00775670055583));
#33725=CARTESIAN_POINT('Ctrl Pts',(-33.0042986476325,-4.10987664439294,
4.60057750330268));
#33726=CARTESIAN_POINT('Ctrl Pts',(-32.8650400035497,-5.81237609034828,
2.06704706776813));
#33727=CARTESIAN_POINT('Ctrl Pts',(-32.7257813594668,-6.09184179716521,
-0.972554838727414));
#33728=CARTESIAN_POINT('Ctrl Pts',(-32.586522715384,-4.87985267103444,-3.77404786734606));
#33729=CARTESIAN_POINT('Ctrl Pts',(-32.4472640713012,-2.47313786215956,
-5.65154744391074));
#33730=CARTESIAN_POINT('Ctrl Pts',(-32.3080054272183,0.539070907307067,
-6.14538867386893));
#33731=CARTESIAN_POINT('Ctrl Pts',(-32.1687467831355,3.41929990172783,-5.13466528393674));
#33732=CARTESIAN_POINT('Ctrl Pts',(-32.0294881390526,5.46238775993218,-2.86683089075102));
#33733=CARTESIAN_POINT('Ctrl Pts',(-31.8902294949698,6.16812890178281,0.102884629624194));
#33734=CARTESIAN_POINT('Ctrl Pts',(-31.750970850887,5.36373797403678,3.04741108843181));
#33735=CARTESIAN_POINT('Ctrl Pts',(-31.6117122068041,3.24615258221831,5.24584529022528));
#33736=CARTESIAN_POINT('Ctrl Pts',(-31.4724535627213,0.333817405615856,
6.15994848482754));
#33737=CARTESIAN_POINT('Ctrl Pts',(-31.3331949186384,-2.66024569490599,
5.56592240682129));
#33738=CARTESIAN_POINT('Ctrl Pts',(-31.1939362745556,-5.00300555568481,
3.6092014083185));
#33739=CARTESIAN_POINT('Ctrl Pts',(-31.0546776304728,-6.12088843118756,
0.768846024230809));
#33740=CARTESIAN_POINT('Ctrl Pts',(-30.9154189863899,-5.74020503780319,
-2.25974456963618));
#33741=CARTESIAN_POINT('Ctrl Pts',(-30.7761603423071,-3.95415741619372,
-4.7350859046042));
#33742=CARTESIAN_POINT('Ctrl Pts',(-30.6369016982242,-1.20002044082553,
-6.05114454773822));
#33743=CARTESIAN_POINT('Ctrl Pts',(-30.4976430541415,1.84791541273056,-5.88571219338953));
#33744=CARTESIAN_POINT('Ctrl Pts',(-30.3583844100586,4.44342941014487,-4.27929135174046));
#33745=CARTESIAN_POINT('Ctrl Pts',(-30.2191257659758,5.95106645847189,-1.62517919100388));
#33746=CARTESIAN_POINT('Ctrl Pts',(-30.0798671218929,6.00171445058094,1.42682271137977));
#33747=CARTESIAN_POINT('Ctrl Pts',(-29.9406084778101,4.58297332830811,4.12949813755107));
#33748=CARTESIAN_POINT('Ctrl Pts',(-29.8013498337272,2.04219096672461,5.82115585184332));
#33749=CARTESIAN_POINT('Ctrl Pts',(-29.6620911896444,-0.998577390644394,
6.08763029354732));
#33750=CARTESIAN_POINT('Ctrl Pts',(-29.5228325455615,-3.79486581486051,
4.86368099727195));
#33751=CARTESIAN_POINT('Ctrl Pts',(-29.3835739014788,-5.66206396582044,
2.44896530048487));
#33752=CARTESIAN_POINT('Ctrl Pts',(-29.2443152573959,-6.14302902874915,
-0.56532623145096));
#33753=CARTESIAN_POINT('Ctrl Pts',(-29.105056613313,-5.12000717952109,-3.44120994385313));
#33754=CARTESIAN_POINT('Ctrl Pts',(-28.9657979692302,-2.8434630447706,-5.47458832324816));
#33755=CARTESIAN_POINT('Ctrl Pts',(-28.8265393251474,0.129241108843973,
-6.16763294399124));
#33756=CARTESIAN_POINT('Ctrl Pts',(-28.6872806810645,3.07030339078509,-5.35066691960496));
#33757=CARTESIAN_POINT('Ctrl Pts',(-28.5480220369817,5.2596687338902,-3.22370659424195));
#33758=CARTESIAN_POINT('Ctrl Pts',(-28.4087633928988,6.16131870058569,-0.307491895558727));
#33759=CARTESIAN_POINT('Ctrl Pts',(-28.2695047488161,5.5545039271765,2.68400549906331));
#33760=CARTESIAN_POINT('Ctrl Pts',(-28.1302461047331,3.58778979940956,5.01838258319093));
#33761=CARTESIAN_POINT('Ctrl Pts',(-27.9909874606504,0.742683452327253,
6.124117951645));
#33762=CARTESIAN_POINT('Ctrl Pts',(-27.8517288165675,-2.28425276841313,
5.73049637344079));
#33763=CARTESIAN_POINT('Ctrl Pts',(-27.7124701724847,-4.75193943137455,
3.93388752210442));
#33764=CARTESIAN_POINT('Ctrl Pts',(-27.5732115284019,-6.05621718340592,
1.17415195926256));
#33765=CARTESIAN_POINT('Ctrl Pts',(-27.433952884319,-5.87776201355233,-1.873049147263));
#33766=CARTESIAN_POINT('Ctrl Pts',(-27.2946942402362,-4.26026478484084,
-4.46167494995614));
#33767=CARTESIAN_POINT('Ctrl Pts',(-27.1554355961533,-1.59973447770233,
-5.95795678037964));
#33768=CARTESIAN_POINT('Ctrl Pts',(-27.0161769520705,1.45245598701167,-5.99556260928159));
#33769=CARTESIAN_POINT('Ctrl Pts',(-26.8769183079876,4.14904422606042,-4.56528546820633));
#33770=CARTESIAN_POINT('Ctrl Pts',(-26.7376596639048,5.82982931901441,-2.01729757526773));
#33771=CARTESIAN_POINT('Ctrl Pts',(-26.598401019822,6.0833076297814,1.02458170853503));
#33772=CARTESIAN_POINT('Ctrl Pts',(-26.4591423757391,4.84742051267944,3.81561446811331));
#33773=CARTESIAN_POINT('Ctrl Pts',(-26.3198837316563,2.42474802069631,5.67247709842451));
#33774=CARTESIAN_POINT('Ctrl Pts',(-26.1806250875734,-0.591571232736088,
6.14055721190029));
#33775=CARTESIAN_POINT('Ctrl Pts',(-26.0413664434907,-3.4630571494742,5.10525558375845));
#33776=CARTESIAN_POINT('Ctrl Pts',(-25.9021077994078,-5.48668892056439,
2.82004327714613));
#33777=CARTESIAN_POINT('Ctrl Pts',(-25.762849155325,-6.167024365203,-0.155595228120675));
#33778=CARTESIAN_POINT('Ctrl Pts',(-25.6235905112421,-5.33749816197862,
-3.09313962938889));
#33779=CARTESIAN_POINT('Ctrl Pts',(-25.4843318671593,-3.20120174137321,
-5.27339613598772));
#33780=CARTESIAN_POINT('Ctrl Pts',(-25.3450732230764,-0.281160770698653,
-6.16257641064526));
#33781=CARTESIAN_POINT('Ctrl Pts',(-25.2058145789936,2.70771629327186,-5.54298402227278));
#33782=CARTESIAN_POINT('Ctrl Pts',(-25.0665559349107,5.03366797501545,-3.56631267744781));
#33783=CARTESIAN_POINT('Ctrl Pts',(-24.927297290828,6.12723564568964,-0.716507319021675));
#33784=CARTESIAN_POINT('Ctrl Pts',(-24.7880386467451,5.72068307019689,2.30871925672743));
#33785=CARTESIAN_POINT('Ctrl Pts',(-24.6487800026623,3.91354579521671,4.76870618771622));
#33786=CARTESIAN_POINT('Ctrl Pts',(-24.5095213585794,1.14826203768109,6.06117923252906));
#33787=CARTESIAN_POINT('Ctrl Pts',(-24.3702627144966,-1.89814867991221,
5.8697045057625));
#33788=CARTESIAN_POINT('Ctrl Pts',(-24.2310040704137,-4.47983901956898,
4.24116042549305));
#33789=CARTESIAN_POINT('Ctrl Pts',(-24.0917454263309,-5.96473830997809,
1.57426055324427));
#33790=CARTESIAN_POINT('Ctrl Pts',(-23.9524867822481,-5.98930128899039,
-1.47806274079266));
#33791=CARTESIAN_POINT('Ctrl Pts',(-23.8132281381652,-4.54751424597783,
-4.16851455300926));
#33792=CARTESIAN_POINT('Ctrl Pts',(-23.6739694940824,-1.99236734795095,
-5.83839633348404));
#33793=CARTESIAN_POINT('Ctrl Pts',(-23.5347108499996,1.05056731756053,-6.07887388479931));
#33794=CARTESIAN_POINT('Ctrl Pts',(-23.3954522059167,3.83629344823421,-4.83107151417328));
#33795=CARTESIAN_POINT('Ctrl Pts',(-23.2561935618339,5.68278665157923,-2.40048646500123));
#33796=CARTESIAN_POINT('Ctrl Pts',(-23.1169349177511,6.13797326845765,0.617805431928693));
#33797=CARTESIAN_POINT('Ctrl Pts',(-22.9776762736682,5.09041076601307,3.48484111966091));
#33798=CARTESIAN_POINT('Ctrl Pts',(-22.8384176295854,2.79657201552275,5.49868933092388));
#33799=CARTESIAN_POINT('Ctrl Pts',(-22.6991589855025,-0.181946506227972,
6.16630317653071));
#33800=CARTESIAN_POINT('Ctrl Pts',(-22.5599003414197,-3.1159193872535,5.32423194161931));
#33801=CARTESIAN_POINT('Ctrl Pts',(-22.4206416973369,-5.28702724585551,
3.17863843455068));
#33802=CARTESIAN_POINT('Ctrl Pts',(-22.281383053254,-6.16372159204044,0.254824511841945));
#33803=CARTESIAN_POINT('Ctrl Pts',(-22.1421244091712,-5.53136290246361,
-2.73137764457251));
#33804=CARTESIAN_POINT('Ctrl Pts',(-22.0028657650883,-3.54477043460551,
-5.04886145204716));
#33805=CARTESIAN_POINT('Ctrl Pts',(-21.8636071210055,-0.690318102290196,
-6.13024145639238));
#33806=CARTESIAN_POINT('Ctrl Pts',(-21.7243484769227,2.33314358782091,-5.71076530726238));
#33807=CARTESIAN_POINT('Ctrl Pts',(-21.5850898328398,4.78538586746803,-3.89313260697071));
#33808=CARTESIAN_POINT('Ctrl Pts',(-21.445831188757,6.0660306045006,-1.12235114883137));
#33809=CARTESIAN_POINT('Ctrl Pts',(-21.3065725446741,5.86153981715024,1.92321355236066));
#33810=CARTESIAN_POINT('Ctrl Pts',(-21.1673139005913,4.22197862254263,4.49792128730755));
#33811=CARTESIAN_POINT('Ctrl Pts',(-21.0280552565085,1.54875788278341,5.97141092343657));
#33812=CARTESIAN_POINT('Ctrl Pts',(-20.8887966124256,-1.50364250514358,
5.98293060403901));
#33813=CARTESIAN_POINT('Ctrl Pts',(-20.7495379683428,-4.18790876286945,
4.52965998612505));
#33814=CARTESIAN_POINT('Ctrl Pts',(-20.61027932426,-5.84685673881853,1.96740074000022));
#33815=CARTESIAN_POINT('Ctrl Pts',(-20.4710206801771,-6.07432913956122,
-1.07653374322349));
#33816=CARTESIAN_POINT('Ctrl Pts',(-20.3317620360943,-4.81463430028632,
-3.85690237762481));
#33817=CARTESIAN_POINT('Ctrl Pts',(-20.1925033920115,-2.37618107641586,
-5.69299243703208));
#33818=CARTESIAN_POINT('Ctrl Pts',(-20.0532447479286,0.644028349992261,
-6.13527724560409));
#33819=CARTESIAN_POINT('Ctrl Pts',(-19.9139861038458,3.50656145663806,-5.07547299735125));
#33820=CARTESIAN_POINT('Ctrl Pts',(-19.7747274597629,5.5105893351992,-2.7730496884856));
#33821=CARTESIAN_POINT('Ctrl Pts',(-19.6354688156801,6.16546939114328,0.208294461991614));
#33822=CARTESIAN_POINT('Ctrl Pts',(-19.4962101715973,5.31086850076819,3.13864224842042));
#33823=CARTESIAN_POINT('Ctrl Pts',(-19.3569515275144,3.15601708578056,5.30056181458931));
#33824=CARTESIAN_POINT('Ctrl Pts',(-19.2176928834316,0.228483599888984,
6.16475422386026));
#33825=CARTESIAN_POINT('Ctrl Pts',(-19.0784342393487,-2.75498912090891,
5.5196407799507));
#33826=CARTESIAN_POINT('Ctrl Pts',(-18.9391755952659,-5.06396273685321,
3.52316346424397));
#33827=CARTESIAN_POINT('Ctrl Pts',(-18.7999169511831,-6.13313532886714,
0.664116280347789));
#33828=CARTESIAN_POINT('Ctrl Pts',(-18.6606583071002,-5.70074326573555,
-2.35752531570539));
#33829=CARTESIAN_POINT('Ctrl Pts',(-18.5213996630174,-3.87264833011119,
-4.80197816605908));
#33830=CARTESIAN_POINT('Ctrl Pts',(-18.3821410189346,-1.09641976584618,
-6.0707712107345));
#33831=CARTESIAN_POINT('Ctrl Pts',(-18.2428823748517,1.94824330692361,-5.85326809680273));
#33832=CARTESIAN_POINT('Ctrl Pts',(-18.1036237307689,4.51592142298934,-4.20271972624959));
#33833=CARTESIAN_POINT('Ctrl Pts',(-17.964365086686,5.977974498913,-1.52322693199904));
#33834=CARTESIAN_POINT('Ctrl Pts',(-17.8251064426032,5.97645067075632,1.52919481297753));
#33835=CARTESIAN_POINT('Ctrl Pts',(-17.6858477985204,4.51172301466689,4.20722650150267));
#33836=CARTESIAN_POINT('Ctrl Pts',(-17.5465891544375,1.94239820730572,5.85521038053091));
#33837=CARTESIAN_POINT('Ctrl Pts',(-17.4073305103547,-1.10248051137719,
6.06967347705416));
#33838=CARTESIAN_POINT('Ctrl Pts',(-17.2680718662719,-3.87744087996609,
4.798109171162));
#33839=CARTESIAN_POINT('Ctrl Pts',(-17.128813222189,-5.70309426842532,2.35183229875672));
#33840=CARTESIAN_POINT('Ctrl Pts',(-16.9895545781062,-6.13246919256903,
-0.670239508096043));
#33841=CARTESIAN_POINT('Ctrl Pts',(-16.8502959340233,-5.06044255053681,
-3.52821776379204));
#33842=CARTESIAN_POINT('Ctrl Pts',(-16.7110372899405,-2.74947672555259,
-5.52238871609615));
#33843=CARTESIAN_POINT('Ctrl Pts',(-16.5717786458577,0.234638614297742,
-6.16452302426568));
#33844=CARTESIAN_POINT('Ctrl Pts',(-16.4325200017748,3.16130779797019,-5.29740808344175));
#33845=CARTESIAN_POINT('Ctrl Pts',(-16.293261357692,5.31399959504801,-3.13333810812859));
#33846=CARTESIAN_POINT('Ctrl Pts',(-16.1540027136092,6.16567428724885,-0.202138515824657));
#33847=CARTESIAN_POINT('Ctrl Pts',(-16.0147440695263,5.50781786877998,2.77855029113547));
#33848=CARTESIAN_POINT('Ctrl Pts',(-15.8754854254435,3.50149216090672,5.07897155368388));
#33849=CARTESIAN_POINT('Ctrl Pts',(-15.7362267813607,0.637902331640281,
6.13591721027176));
#33850=CARTESIAN_POINT('Ctrl Pts',(-15.5969681372778,-2.38186399517015,
5.69061712861911));
#33851=CARTESIAN_POINT('Ctrl Pts',(-15.457709493195,-4.81848278051395,3.85209333868117));
#33852=CARTESIAN_POINT('Ctrl Pts',(-15.3184508491121,-6.07540096466732,
1.0704683622325));
#33853=CARTESIAN_POINT('Ctrl Pts',(-15.1791922050293,-5.84488949576155,
-1.97323748655797));
#33854=CARTESIAN_POINT('Ctrl Pts',(-15.0399335609465,-4.18338408828115,
-4.53383909793204));
#33855=CARTESIAN_POINT('Ctrl Pts',(-14.9006749168636,-1.4976681670861,-5.98442891655653));
#33856=CARTESIAN_POINT('Ctrl Pts',(-14.7614162727808,1.55471919770946,-5.96986160746585));
#33857=CARTESIAN_POINT('Ctrl Pts',(-14.6221576286979,4.22646741616687,-4.49370365913252));
#33858=CARTESIAN_POINT('Ctrl Pts',(-14.4828989846151,5.8634571060835,-1.9173602064141));
#33859=CARTESIAN_POINT('Ctrl Pts',(-14.3436403405323,6.06490698229064,1.12840714823311));
#33860=CARTESIAN_POINT('Ctrl Pts',(-14.2043816964494,4.78149642854946,3.89790858022476));
#33861=CARTESIAN_POINT('Ctrl Pts',(-14.0651230523666,2.32744057663251,5.71309196129958));
#33862=CARTESIAN_POINT('Ctrl Pts',(-13.9258644082838,-0.696438427624502,
6.1295491606275));
#33863=CARTESIAN_POINT('Ctrl Pts',(-13.7866057642009,-3.54980964567892,
5.04531970002558));
#33864=CARTESIAN_POINT('Ctrl Pts',(-13.6473471201181,-5.53408725815802,
2.72585355716592));
#33865=CARTESIAN_POINT('Ctrl Pts',(-13.5080884760353,-6.16346409317852,
-0.26097848210198));
#33866=CARTESIAN_POINT('Ctrl Pts',(-13.3688298319524,-5.28385093542735,
-3.18391562202968));
#33867=CARTESIAN_POINT('Ctrl Pts',(-13.2295711878696,-3.11060191571313,
-5.32734034185756));
#33868=CARTESIAN_POINT('Ctrl Pts',(-13.0903125437867,-0.175789740710468,
-6.16648176540581));
#33869=CARTESIAN_POINT('Ctrl Pts',(-12.9510538997039,2.80206072502511,-5.49589438483793));
#33870=CARTESIAN_POINT('Ctrl Pts',(-12.811795255621,5.09388762847827,-3.47975692031169));
#33871=CARTESIAN_POINT('Ctrl Pts',(-12.6725366115382,6.1385870498091,-0.61167673483411));
#33872=CARTESIAN_POINT('Ctrl Pts',(-12.5332779674554,5.68038708081621,2.40615918179108));
#33873=CARTESIAN_POINT('Ctrl Pts',(-12.3940193233725,3.83146800801478,4.83489940945832));
#33874=CARTESIAN_POINT('Ctrl Pts',(-12.2547606792897,1.04449741186333,6.07991978175963));
#33875=CARTESIAN_POINT('Ctrl Pts',(-12.1155020352069,-1.99819563486947,
5.83640416702013));
#33876=CARTESIAN_POINT('Ctrl Pts',(-11.9762433911241,-4.55167398495864,
4.16397206170644));
#33877=CARTESIAN_POINT('Ctrl Pts',(-11.8369847470412,-5.99077405850954,
1.47208205474779));
#33878=CARTESIAN_POINT('Ctrl Pts',(-11.6977261029584,-5.9631635344839,-1.58021519326419));
#33879=CARTESIAN_POINT('Ctrl Pts',(-11.5584674588755,-4.47560224855524,
-4.24563115552312));
#33880=CARTESIAN_POINT('Ctrl Pts',(-11.4192088147927,-1.89228719451897,
-5.87159676489119));
#33881=CARTESIAN_POINT('Ctrl Pts',(-11.2799501707098,1.15431318037104,-6.06002974230678));
#33882=CARTESIAN_POINT('Ctrl Pts',(-11.140691526627,3.91830510466066,-4.76479637579732));
#33883=CARTESIAN_POINT('Ctrl Pts',(-11.0014328825442,5.72298533309686,-2.30300635543621));
#33884=CARTESIAN_POINT('Ctrl Pts',(-10.8621742384613,6.12651720309929,0.72262463018494));
#33885=CARTESIAN_POINT('Ctrl Pts',(-10.7229155943785,5.03010472196112,3.57133670803045));
#33886=CARTESIAN_POINT('Ctrl Pts',(-10.5836569502956,2.70218061468502,5.54568474776935));
#33887=CARTESIAN_POINT('Ctrl Pts',(-10.4443983062128,-0.287313584438326,
6.16229261721792));
#33888=CARTESIAN_POINT('Ctrl Pts',(-10.30513966213,-3.2064653077802,5.27019730427842));
#33889=CARTESIAN_POINT('Ctrl Pts',(-10.1658810180471,-5.34058381141607,
3.08780892369685));
#33890=CARTESIAN_POINT('Ctrl Pts',(-10.0266223739643,-6.16717664358659,
0.149437755674944));
#33891=CARTESIAN_POINT('Ctrl Pts',(-9.88736372988148,-5.48387054584736,
-2.82551999327713));
#33892=CARTESIAN_POINT('Ctrl Pts',(-9.74810508579863,-3.45795813934461,
-5.10871068886872));
#33893=CARTESIAN_POINT('Ctrl Pts',(-9.6088464417158,-0.585439968808977,
-6.14114479872785));
#33894=CARTESIAN_POINT('Ctrl Pts',(-9.46958779763296,2.43041043193784,-5.67005330912764));
#33895=CARTESIAN_POINT('Ctrl Pts',(-9.33032915355013,4.8512277531245,-3.81077271473068));
#33896=CARTESIAN_POINT('Ctrl Pts',(-9.19107050946727,6.08432757949787,-1.01850738896811));
#33897=CARTESIAN_POINT('Ctrl Pts',(-9.05181186538446,5.82781226552048,2.0231172961226));
#33898=CARTESIAN_POINT('Ctrl Pts',(-8.9125532213016,4.14448400098889,4.56942575840426));
#33899=CARTESIAN_POINT('Ctrl Pts',(-8.77329457721878,1.44646906218654,5.99700980890963));
#33900=CARTESIAN_POINT('Ctrl Pts',(-8.63403593313592,-1.60568233408446,
5.9563565741173));
#33901=CARTESIAN_POINT('Ctrl Pts',(-8.49477728905311,-4.26471736964113,
4.45741911346718));
#33902=CARTESIAN_POINT('Ctrl Pts',(-8.35551864497025,-5.8796292083237,1.86717962945399));
#33903=CARTESIAN_POINT('Ctrl Pts',(-8.21626000088743,-6.05504184616107,
-1.18019813474674));
#33904=CARTESIAN_POINT('Ctrl Pts',(-8.07700135680458,-4.74800931784848,
-3.93863008083336));
#33905=CARTESIAN_POINT('Ctrl Pts',(-7.93774271272175,-2.27853008133649,
-5.7327742031643));
#33906=CARTESIAN_POINT('Ctrl Pts',(-7.79848406863889,0.748797637617561,
-6.12337337534789));
#33907=CARTESIAN_POINT('Ctrl Pts',(-7.65922542455608,3.59279855776266,-5.01479789416878));
#33908=CARTESIAN_POINT('Ctrl Pts',(-7.51996678047323,5.55718097315999,-2.67845833037771));
#33909=CARTESIAN_POINT('Ctrl Pts',(-7.3807081363904,6.16100861777501,0.313643440427673));
#33910=CARTESIAN_POINT('Ctrl Pts',(-7.24144949230756,5.25644743931043,3.22895644346409));
#33911=CARTESIAN_POINT('Ctrl Pts',(-7.10219084822472,3.06495954828024,5.3537297618975));
#33912=CARTESIAN_POINT('Ctrl Pts',(-6.96293220414188,0.12308304190572,6.16775890910275));
#33913=CARTESIAN_POINT('Ctrl Pts',(-6.82367356005905,-2.84892766752535,
5.47174657136365));
#33914=CARTESIAN_POINT('Ctrl Pts',(-6.68441491597621,-5.12344046418626,
3.43609621605106));
#33915=CARTESIAN_POINT('Ctrl Pts',(-6.54515627189336,-6.14359041032356,
0.55919251264796));
#33916=CARTESIAN_POINT('Ctrl Pts',(-6.40589762781053,-5.65961600224796,
-2.45461730278265));
#33917=CARTESIAN_POINT('Ctrl Pts',(-6.2666389837277,-3.79000783672504,-4.86746751335681));
#33918=CARTESIAN_POINT('Ctrl Pts',(-6.12738033964486,-0.992498768124922,
-6.08862427739564));
#33919=CARTESIAN_POINT('Ctrl Pts',(-5.98812169556202,2.04800201524751,-5.81911394815082));
#33920=CARTESIAN_POINT('Ctrl Pts',(-5.84886305147919,4.58709409412132,-4.12492026198068));
#33921=CARTESIAN_POINT('Ctrl Pts',(-5.70960440739633,6.00313605389204,-1.42082965709572));
#33922=CARTESIAN_POINT('Ctrl Pts',(-5.5703457633135,5.94944085066117,1.6311201551404));
#33923=CARTESIAN_POINT('Ctrl Pts',(-5.43108711923068,4.4391545858922,4.28372571000683));
#33924=CARTESIAN_POINT('Ctrl Pts',(-5.29182847514783,1.84203796968307,5.88755428970869));
#33925=CARTESIAN_POINT('Ctrl Pts',(-5.15256983106499,-1.20606153870089,
6.04994338493243));
#33926=CARTESIAN_POINT('Ctrl Pts',(-5.01331118698216,-3.95888313760845,
4.7311355612348));
#33927=CARTESIAN_POINT('Ctrl Pts',(-4.87405254289932,-5.74245839275694,
2.25401220127068));
#33928=CARTESIAN_POINT('Ctrl Pts',(-4.73479389881648,-6.12011773477969,
-0.774956972002906));
#33929=CARTESIAN_POINT('Ctrl Pts',(-4.59553525473365,-4.99939949615145,
-3.61419480298191));
#33930=CARTESIAN_POINT('Ctrl Pts',(-4.45627661065081,-2.65468713741269,
-5.56857572440924));
#33931=CARTESIAN_POINT('Ctrl Pts',(-4.31701796656796,0.339967569286781,
-6.15961211829499));
#33932=CARTESIAN_POINT('Ctrl Pts',(-4.17775932248513,3.251388618394,-5.24260159159703));
#33933=CARTESIAN_POINT('Ctrl Pts',(-4.0385006784023,5.36677795325581,-3.04205420669029));
#33934=CARTESIAN_POINT('Ctrl Pts',(-3.89924203431946,6.1682285513242,-0.0967260806445108));
#33935=CARTESIAN_POINT('Ctrl Pts',(-3.75998339023662,5.45952268276649,2.87228332035471));
#33936=CARTESIAN_POINT('Ctrl Pts',(-3.62072474615379,3.41417154963807,5.13807668544686));
#33937=CARTESIAN_POINT('Ctrl Pts',(-3.48146610207094,0.532934845614573,
6.14592383997453));
#33938=CARTESIAN_POINT('Ctrl Pts',(-3.3422074579881,-2.47877935227735,5.64907535069391));
#33939=CARTESIAN_POINT('Ctrl Pts',(-3.20294881390527,-4.88361839367658,
3.76917375329861));
#33940=CARTESIAN_POINT('Ctrl Pts',(-3.06369016982243,-6.09280979687953,
0.966472023989456));
#33941=CARTESIAN_POINT('Ctrl Pts',(-2.92443152573958,-5.81030937396819,
-2.07284933733924));
#33942=CARTESIAN_POINT('Ctrl Pts',(-2.78517288165675,-4.10528120147494,
-4.60467867048159));
#33943=CARTESIAN_POINT('Ctrl Pts',(-2.64591423757392,-1.39516430851072,
-6.00915267964906));
#33944=CARTESIAN_POINT('Ctrl Pts',(-2.50665559349108,1.65652819361447,-5.94241649418644));
#33945=CARTESIAN_POINT('Ctrl Pts',(-2.36739694940825,4.30265582625509,-4.42080899194675));
#33946=CARTESIAN_POINT('Ctrl Pts',(-2.22813830532541,5.89537187071915,-1.81686268871946));
#33947=CARTESIAN_POINT('Ctrl Pts',(-2.08887966124256,6.0447344392611,1.23190294811429));
#33948=CARTESIAN_POINT('Ctrl Pts',(-1.94962101715973,4.71417543837697,3.97906385024911));
#33949=CARTESIAN_POINT('Ctrl Pts',(-1.81036237307689,2.22945311551249,5.75203783218659));
#33950=CARTESIAN_POINT('Ctrl Pts',(-1.67110372899405,-0.801102063147124,
6.11675013179543));
#33951=CARTESIAN_POINT('Ctrl Pts',(-1.53184508491122,-3.63552523351456,
4.98391021694912));
#33952=CARTESIAN_POINT('Ctrl Pts',(-1.39258644082839,-5.57986844123835,
2.6308666740793));
#33953=CARTESIAN_POINT('Ctrl Pts',(-1.25332779674554,-6.15810383146443,
-0.366283937729162));
#33954=CARTESIAN_POINT('Ctrl Pts',(-1.1140691526627,-5.22865867321571,-3.27376445220254));
#33955=CARTESIAN_POINT('Ctrl Pts',(-0.974810508579875,-3.01909593307338,
-5.37972223694837));
#33956=CARTESIAN_POINT('Ctrl Pts',(-0.835551864497024,-0.0703622493363052,
-6.16859709325572));
#33957=CARTESIAN_POINT('Ctrl Pts',(-0.696293220414186,2.89557656689768,
-5.44717660208643));
#33958=CARTESIAN_POINT('Ctrl Pts',(-0.557034576331352,5.15263851981499,
-3.3922284657316));
#33959=CARTESIAN_POINT('Ctrl Pts',(-0.417775932248521,6.14810707551576,
-0.50658149428877));
#33960=CARTESIAN_POINT('Ctrl Pts',(-0.278517288165677,5.63850617107878,
2.50272579507521));
#33961=CARTESIAN_POINT('Ctrl Pts',(-0.139258644082849,3.74811954234602,
4.90004022087069));
#33962=CARTESIAN_POINT('Ctrl Pts',(-0.046419548027623,1.87656122511999,
5.69726812402409));
#33963=CARTESIAN_POINT('Ctrl Pts',(-8.88178419700125E-15,0.901975524283881,
5.84759529345977));
#33964=CARTESIAN_POINT('Ctrl Pts',(-59.9675728291906,3.24375760296871,-4.54512507566739));
#33965=CARTESIAN_POINT('Ctrl Pts',(-59.9211532811629,4.00126794439251,-4.00450630535553));
#33966=CARTESIAN_POINT('Ctrl Pts',(-59.8283141851077,5.2399731520367,-2.53773238462263));
#33967=CARTESIAN_POINT('Ctrl Pts',(-59.6890555410249,5.8149566612005,0.285552748802543));
#33968=CARTESIAN_POINT('Ctrl Pts',(-59.549796896942,4.96632117772543,3.0381625750435));
#33969=CARTESIAN_POINT('Ctrl Pts',(-59.4105382528592,2.90177043637895,5.0473204187532));
#33970=CARTESIAN_POINT('Ctrl Pts',(-59.2712796087763,0.126794047904731,
5.820560526789));
#33971=CARTESIAN_POINT('Ctrl Pts',(-59.1320209646935,-2.67923001924639,
5.16886098189645));
#33972=CARTESIAN_POINT('Ctrl Pts',(-58.9927623206107,-4.82930043184711,
3.25162821416299));
#33973=CARTESIAN_POINT('Ctrl Pts',(-58.8535036765279,-5.79702306621662,
0.538330773663447));
#33974=CARTESIAN_POINT('Ctrl Pts',(-58.714245032445,-5.3454701543225,-2.30677840908288));
#33975=CARTESIAN_POINT('Ctrl Pts',(-58.5749863883622,-3.58519559498042,
-4.58711636978122));
#33976=CARTESIAN_POINT('Ctrl Pts',(-58.4357277442793,-0.947163777203368,
-5.74440221811722));
#33977=CARTESIAN_POINT('Ctrl Pts',(-58.2964691001966,1.92276038087513,-5.49529447639017));
#33978=CARTESIAN_POINT('Ctrl Pts',(-58.1572104561136,4.32193856748268,-3.9007844342772));
#33979=CARTESIAN_POINT('Ctrl Pts',(-58.0179518120309,5.66298416936691,-1.3512517850711));
#33980=CARTESIAN_POINT('Ctrl Pts',(-57.878693167948,5.61757140339575,1.52910520556));
#33981=CARTESIAN_POINT('Ctrl Pts',(-57.7394345238651,4.19681857847456,4.03509420056188));
#33982=CARTESIAN_POINT('Ctrl Pts',(-57.6001758797823,1.74856610055642,5.5531781695683));
#33983=CARTESIAN_POINT('Ctrl Pts',(-57.4609172356995,-1.12778471905584,
5.71168739925639));
#33984=CARTESIAN_POINT('Ctrl Pts',(-57.3216585916167,-3.7280220034185,4.47181430715398));
#33985=CARTESIAN_POINT('Ctrl Pts',(-57.1823999475338,-5.41553426686218,
2.13711485037188));
#33986=CARTESIAN_POINT('Ctrl Pts',(-57.043141303451,-5.77717087142268,-0.720810652760878));
#33987=CARTESIAN_POINT('Ctrl Pts',(-56.9038826593682,-4.72439296832481,
-3.40226135877762));
#33988=CARTESIAN_POINT('Ctrl Pts',(-56.7646240152853,-2.51495030597815,
-5.25074244599479));
#33989=CARTESIAN_POINT('Ctrl Pts',(-56.6253653712025,0.310223183462825,
-5.81369356346818));
#33990=CARTESIAN_POINT('Ctrl Pts',(-56.4861067271197,3.05944528060205,-4.95328838749244));
#33991=CARTESIAN_POINT('Ctrl Pts',(-56.3468480830367,5.05962881077401,-2.88017839228123));
#33992=CARTESIAN_POINT('Ctrl Pts',(-56.207589438954,5.82107238446222,-0.101919424810071));
#33993=CARTESIAN_POINT('Ctrl Pts',(-56.0683307948711,5.15735312073121,2.70129229488456));
#33994=CARTESIAN_POINT('Ctrl Pts',(-55.9290721507883,3.2309682308663,4.84315140847404));
#33995=CARTESIAN_POINT('Ctrl Pts',(-55.7898135067055,0.513551114052919,
5.79927034441098));
#33996=CARTESIAN_POINT('Ctrl Pts',(-55.6505548626226,-2.32959781204261,
5.33556419775959));
#33997=CARTESIAN_POINT('Ctrl Pts',(-55.5112962185398,-4.60239543367529,
3.56556132276284));
#33998=CARTESIAN_POINT('Ctrl Pts',(-55.3720375744569,-5.7483967363546,0.922608386999673));
#33999=CARTESIAN_POINT('Ctrl Pts',(-55.2327789303741,-5.48702825176757,
-1.94622512536426));
#34000=CARTESIAN_POINT('Ctrl Pts',(-55.0935202862912,-3.88228036287168,
-4.33856778883955));
#34001=CARTESIAN_POINT('Ctrl Pts',(-54.9542616422084,-1.32704065182156,
-5.6687065881652));
#34002=CARTESIAN_POINT('Ctrl Pts',(-54.8150029981255,1.55309607060505,-5.61098599800124));
#34003=CARTESIAN_POINT('Ctrl Pts',(-54.6757443540427,4.05299103402638,-4.17953764816116));
#34004=CARTESIAN_POINT('Ctrl Pts',(-54.5364857099599,5.56059938416019,-1.72482050172535));
#34005=CARTESIAN_POINT('Ctrl Pts',(-54.397227065877,5.70681604000361,1.15218139190509));
#34006=CARTESIAN_POINT('Ctrl Pts',(-54.2579684217942,4.45584303679061,3.74709675692789));
#34007=CARTESIAN_POINT('Ctrl Pts',(-54.1187097777113,2.11395387827456,5.42461706250522));
#34008=CARTESIAN_POINT('Ctrl Pts',(-53.9794511336286,-0.745490862503697,
5.77403798465323));
#34009=CARTESIAN_POINT('Ctrl Pts',(-53.8401924895457,-3.42241839636484,
4.70981141814811));
#34010=CARTESIAN_POINT('Ctrl Pts',(-53.7009338454629,-5.26144129849329,
2.4924900675437));
#34011=CARTESIAN_POINT('Ctrl Pts',(-53.56167520138,-5.8123148503612,-0.335063209806113));
#34012=CARTESIAN_POINT('Ctrl Pts',(-53.4224165572972,-4.94016965636819,
-3.08058355520409));
#34013=CARTESIAN_POINT('Ctrl Pts',(-53.2831579132143,-2.85853147898867,
-5.07189008732698));
#34014=CARTESIAN_POINT('Ctrl Pts',(-53.1438992691315,-0.0770441046955488,
-5.82145475634969));
#34015=CARTESIAN_POINT('Ctrl Pts',(-53.0046406250486,2.72330584123424,-5.14576297252353));
#34016=CARTESIAN_POINT('Ctrl Pts',(-52.8653819809659,4.85691364353293,-3.21024315801133));
#34017=CARTESIAN_POINT('Ctrl Pts',(-52.726123336883,5.80141188454461,-0.488765199415102));
#34018=CARTESIAN_POINT('Ctrl Pts',(-52.5868646928002,5.32556073349711,2.3523762769014));
#34019=CARTESIAN_POINT('Ctrl Pts',(-52.4476060487173,3.54586198453153,4.61758963756513));
#34020=CARTESIAN_POINT('Ctrl Pts',(-52.3083474046345,0.898036128874486,
5.75228670926015));
#34021=CARTESIAN_POINT('Ctrl Pts',(-52.1690887605517,-1.96965432096735,
5.47866161851501));
#34022=CARTESIAN_POINT('Ctrl Pts',(-52.0298301164688,-4.35511779347528,
3.86370551145526));
#34023=CARTESIAN_POINT('Ctrl Pts',(-51.890571472386,-5.67432549352408,1.30280523020041));
#34024=CARTESIAN_POINT('Ctrl Pts',(-51.7513128283031,-5.6042981374404,-1.57705854709862));
#34025=CARTESIAN_POINT('Ctrl Pts',(-51.6120541842203,-4.16218039873141,
-4.07081387473205));
#34026=CARTESIAN_POINT('Ctrl Pts',(-51.4727955401375,-1.70104340804889,
-5.56791905456861));
#34027=CARTESIAN_POINT('Ctrl Pts',(-51.3335368960546,1.17655702611451,-5.70184047817855));
#34028=CARTESIAN_POINT('Ctrl Pts',(-51.1942782519718,3.76610308833844,-4.43979040071741));
#34029=CARTESIAN_POINT('Ctrl Pts',(-51.055019607889,5.43360080467535,-2.09075430639906));
#34030=CARTESIAN_POINT('Ctrl Pts',(-50.9157609638061,5.77079966390589,0.770157460107026));
#34031=CARTESIAN_POINT('Ctrl Pts',(-50.7765023197233,4.69514386681382,3.44251294031197));
#34032=CARTESIAN_POINT('Ctrl Pts',(-50.6372436756404,2.46998431622591,5.27204407719557));
#34033=CARTESIAN_POINT('Ctrl Pts',(-50.4979850315576,-0.359897117890633,
5.81083000429618));
#34034=CARTESIAN_POINT('Ctrl Pts',(-50.3587263874747,-3.10166557834268,
4.92696071776699));
#34035=CARTESIAN_POINT('Ctrl Pts',(-50.2194677433919,-5.08405875115028,
2.83683236888383));
#34036=CARTESIAN_POINT('Ctrl Pts',(-50.0802090993091,-5.82173082845574,
0.0521673777649718));
#34037=CARTESIAN_POINT('Ctrl Pts',(-49.9409504552262,-5.13407886266778,
-2.7452696600157));
#34038=CARTESIAN_POINT('Ctrl Pts',(-49.8016918111435,-3.18945946610645,
-4.87058719133112));
#34039=CARTESIAN_POINT('Ctrl Pts',(-49.6624331670605,-0.463970359923155,
-5.80344749088054));
#34040=CARTESIAN_POINT('Ctrl Pts',(-49.5231745229778,2.37511178736206,-5.31546002447846));
#34041=CARTESIAN_POINT('Ctrl Pts',(-49.3839158788949,4.63269952425391,-3.52609789884971));
#34042=CARTESIAN_POINT('Ctrl Pts',(-49.2446572348121,5.75607164539254,-0.8734474726066));
#34043=CARTESIAN_POINT('Ctrl Pts',(-49.1053985907293,5.47019494488432,1.99304755067632));
#34044=CARTESIAN_POINT('Ctrl Pts',(-48.9661399466464,3.84506010876424,4.37158827364663));
#34045=CARTESIAN_POINT('Ctrl Pts',(-48.8268813025635,1.27854601935176,5.67984078568181));
#34046=CARTESIAN_POINT('Ctrl Pts',(-48.6876226584807,-1.60099222649822,
5.5975079423782));
#34047=CARTESIAN_POINT('Ctrl Pts',(-48.5483640143979,-4.08856238236371,
4.14474714787467));
#34048=CARTESIAN_POINT('Ctrl Pts',(-48.4091053703151,-5.57513705475781,
1.67723525331457));
#34049=CARTESIAN_POINT('Ctrl Pts',(-48.2698467262321,-5.69676080072868,
-1.20091117638895));
#34050=CARTESIAN_POINT('Ctrl Pts',(-48.1305880821495,-4.42365669405774,
-3.78504065069492));
#34051=CARTESIAN_POINT('Ctrl Pts',(-47.9913294380665,-2.06751655734344,
-5.44248532927793));
#34052=CARTESIAN_POINT('Ctrl Pts',(-47.8520707939837,0.794809994632685,
-5.76745596833879));
#34053=CARTESIAN_POINT('Ctrl Pts',(-47.7128121499008,3.46254462396208,-4.680390582138));
#34054=CARTESIAN_POINT('Ctrl Pts',(-47.5735535058181,5.28255058835662,-2.4474334629869));
#34055=CARTESIAN_POINT('Ctrl Pts',(-47.4342948617351,5.80923905245728,0.384724454252631));
#34056=CARTESIAN_POINT('Ctrl Pts',(-47.2950362176524,4.91366181284781,3.1226909650582));
#34057=CARTESIAN_POINT('Ctrl Pts',(-47.1557775735695,2.81508145821114,5.09613458004502));
#34058=CARTESIAN_POINT('Ctrl Pts',(-47.0165189294867,0.0272896982579126,
5.8219005957388));
#34059=CARTESIAN_POINT('Ctrl Pts',(-46.8772602854038,-2.76718335016466,
5.12230100451606));
#34060=CARTESIAN_POINT('Ctrl Pts',(-46.738001641321,-4.8841718021921,3.16861753466183));
#34061=CARTESIAN_POINT('Ctrl Pts',(-46.5987429972381,-5.80537712624728,
0.439167048330993));
#34062=CARTESIAN_POINT('Ctrl Pts',(-46.4594843531554,-5.30526225514328,
-2.39780392827412));
#34063=CARTESIAN_POINT('Ctrl Pts',(-46.3202257090724,-3.50626942660932,
-4.64772481783502));
#34064=CARTESIAN_POINT('Ctrl Pts',(-46.1809670649897,-0.848842867185158,
-5.75975147563883));
#34065=CARTESIAN_POINT('Ctrl Pts',(-46.0417084209067,2.01640438733086,-5.46162838547696));
#34066=CARTESIAN_POINT('Ctrl Pts',(-45.902449776824,4.38797892860256,-3.82634449526369));
#34067=CARTESIAN_POINT('Ctrl Pts',(-45.7631911327411,5.68525236392919,-1.25426346224879));
#34068=CARTESIAN_POINT('Ctrl Pts',(-45.6239324886583,5.59061553680362,1.62489667177482));
#34069=CARTESIAN_POINT('Ctrl Pts',(-45.4846738445754,4.12723821392213,4.10623623283363));
#34070=CARTESIAN_POINT('Ctrl Pts',(-45.3454152004926,1.65339647225928,5.58225325292712));
#34071=CARTESIAN_POINT('Ctrl Pts',(-45.2061565564098,-1.22524339802163,
5.69157710040891));
#34072=CARTESIAN_POINT('Ctrl Pts',(-45.0668979123269,-3.80390909819738,
4.40744221141311));
#34073=CARTESIAN_POINT('Ctrl Pts',(-44.9276392682442,-5.45127047408152,
2.04424105542907));
#34074=CARTESIAN_POINT('Ctrl Pts',(-44.7883806241612,-5.76400695900782,
-0.819448015925402));
#34075=CARTESIAN_POINT('Ctrl Pts',(-44.6491219800785,-4.66555183351562,
-3.48251308153665));
#34076=CARTESIAN_POINT('Ctrl Pts',(-44.5098633359956,-2.42483791960524,
-5.29296064012754));
#34077=CARTESIAN_POINT('Ctrl Pts',(-44.3706046919128,0.409544765544918,
-5.80754202389527));
#34078=CARTESIAN_POINT('Ctrl Pts',(-44.2313460478299,3.14365933142698,-4.90027318444869));
#34079=CARTESIAN_POINT('Ctrl Pts',(-44.0920874037471,5.1081173535065,-2.79327914414233));
#34080=CARTESIAN_POINT('Ctrl Pts',(-43.9528287596642,5.82196405509893,-0.00241152044091948));
#34081=CARTESIAN_POINT('Ctrl Pts',(-43.8135701155814,5.11042961313214,2.78904651153705));
#34082=CARTESIAN_POINT('Ctrl Pts',(-43.6743114714985,3.1477177442512,4.89766722806082));
#34083=CARTESIAN_POINT('Ctrl Pts',(-43.5350528274158,0.414355717547182,
5.80720075540968));
#34084=CARTESIAN_POINT('Ctrl Pts',(-43.3957941833329,-2.420452285279,5.29496761170287));
#34085=CARTESIAN_POINT('Ctrl Pts',(-43.25653553925,-4.66266524394653,3.48637692987834));
#34086=CARTESIAN_POINT('Ctrl Pts',(-43.1172768951672,-5.76332613280533,
0.824222761890331));
#34087=CARTESIAN_POINT('Ctrl Pts',(-42.9780182510844,-5.45296209671835,
-2.03972440443504));
#34088=CARTESIAN_POINT('Ctrl Pts',(-42.8387596070015,-3.80755901270078,
-4.40428945904965));
#34089=CARTESIAN_POINT('Ctrl Pts',(-42.6995009629187,-1.2299580022911,-5.69056012945078));
#34090=CARTESIAN_POINT('Ctrl Pts',(-42.5602423188358,1.64877144643314,-5.58362104657198));
#34091=CARTESIAN_POINT('Ctrl Pts',(-42.4209836747531,4.12383510341716,-4.10965391658703));
#34092=CARTESIAN_POINT('Ctrl Pts',(-42.2817250306701,5.58926751913469,-1.62952750017931));
#34093=CARTESIAN_POINT('Ctrl Pts',(-42.1424663865874,5.68628947187366,1.24955324670603));
#34094=CARTESIAN_POINT('Ctrl Pts',(-42.0032077425045,4.39114724886002,3.82270808630791));
#34095=CARTESIAN_POINT('Ctrl Pts',(-41.8639490984217,2.02092822566666,5.45995607866938));
#34096=CARTESIAN_POINT('Ctrl Pts',(-41.7246904543388,-0.844071074094882,
5.76045269889192));
#34097=CARTESIAN_POINT('Ctrl Pts',(-41.585431810256,-3.50241794841162,4.65062789190223));
#34098=CARTESIAN_POINT('Ctrl Pts',(-41.4461731661731,-5.3032740424208,2.40219809867558));
#34099=CARTESIAN_POINT('Ctrl Pts',(-41.3069145220903,-5.80573894959788,
-0.434357598548544));
#34100=CARTESIAN_POINT('Ctrl Pts',(-41.1676558780075,-4.88679507704601,
-3.16457029456666));
#34101=CARTESIAN_POINT('Ctrl Pts',(-41.0283972339247,-2.77142582478762,
-5.1200068527293));
#34102=CARTESIAN_POINT('Ctrl Pts',(-40.8891385898418,0.0224667014105143,
-5.82192120537735));
#34103=CARTESIAN_POINT('Ctrl Pts',(-40.749879945759,2.81085874491149,-5.09846490528761));
#34104=CARTESIAN_POINT('Ctrl Pts',(-40.6106213016761,4.91107322251077,-3.1267604765048));
#34105=CARTESIAN_POINT('Ctrl Pts',(-40.4713626575933,5.80891834506829,-0.389536820626648));
#34106=CARTESIAN_POINT('Ctrl Pts',(-40.3321040135105,5.28457628213744,2.44305644481769));
#34107=CARTESIAN_POINT('Ctrl Pts',(-40.1928453694276,3.46642077189376,4.67752052977624));
#34108=CARTESIAN_POINT('Ctrl Pts',(-40.0535867253448,0.799587606285317,
5.76679555161875));
#34109=CARTESIAN_POINT('Ctrl Pts',(-39.9143280812619,-2.06300717616523,
5.44419623685495));
#34110=CARTESIAN_POINT('Ctrl Pts',(-39.7750694371791,-4.42051956715754,
3.78870400409851));
#34111=CARTESIAN_POINT('Ctrl Pts',(-39.6358107930963,-5.69576398532674,
1.20563008329652));
#34112=CARTESIAN_POINT('Ctrl Pts',(-39.4965521490134,-5.57652459940273,
-1.67261611451975));
#34113=CARTESIAN_POINT('Ctrl Pts',(-39.3572935049306,-4.09199457695864,
-4.14135867275896));
#34114=CARTESIAN_POINT('Ctrl Pts',(-39.2180348608478,-1.60562877292209,
-5.59617972530006));
#34115=CARTESIAN_POINT('Ctrl Pts',(-39.0787762167649,1.27384027854431,-5.68089801167499));
#34116=CARTESIAN_POINT('Ctrl Pts',(-38.9395175726821,3.84143727175693,-4.37477210394456));
#34117=CARTESIAN_POINT('Ctrl Pts',(-38.8002589285993,5.46854198444228,-1.9975784937486));
#34118=CARTESIAN_POINT('Ctrl Pts',(-38.6610002845164,5.75679325289186,0.868678719523871));
#34119=CARTESIAN_POINT('Ctrl Pts',(-38.5217416404336,4.63561902980916,3.52225886112391));
#34120=CARTESIAN_POINT('Ctrl Pts',(-38.3824829963507,2.37951441360128,5.31349060691355));
#34121=CARTESIAN_POINT('Ctrl Pts',(-38.2432243522679,-0.459162500181017,
5.80382986248928));
#34122=CARTESIAN_POINT('Ctrl Pts',(-38.1039657081851,-3.18542347264294,
4.87322773675008));
#34123=CARTESIAN_POINT('Ctrl Pts',(-37.9647070641022,-5.1318028606111,2.74952189918877));
#34124=CARTESIAN_POINT('Ctrl Pts',(-37.8254484200194,-5.82177204735652,
-0.0473445130199082));
#34125=CARTESIAN_POINT('Ctrl Pts',(-37.6861897759365,-5.08640709945809,
-2.83261965199657));
#34126=CARTESIAN_POINT('Ctrl Pts',(-37.5469311318537,-3.1057461141024,-4.92438954074844));
#34127=CARTESIAN_POINT('Ctrl Pts',(-37.4076724877709,-0.364710810762607,
-5.8105298638599));
#34128=CARTESIAN_POINT('Ctrl Pts',(-37.2684138436881,2.46561599413806,-5.27408845619272));
#34129=CARTESIAN_POINT('Ctrl Pts',(-37.1291551996052,4.69229040406655,-3.4464013170552));
#34130=CARTESIAN_POINT('Ctrl Pts',(-36.9898965555224,5.77015966872752,-0.774937850208125));
#34131=CARTESIAN_POINT('Ctrl Pts',(-36.8506379114395,5.43533096595136,2.08625227737804));
#34132=CARTESIAN_POINT('Ctrl Pts',(-36.7113792673567,3.76977981374935,4.43666895656445));
#34133=CARTESIAN_POINT('Ctrl Pts',(-36.5721206232738,1.18128014949281,5.70086383653468));
#34134=CARTESIAN_POINT('Ctrl Pts',(-36.432861979191,-1.69643024063091,5.56932632487699));
#34135=CARTESIAN_POINT('Ctrl Pts',(-36.2936033351081,-4.15880662087851,
4.07426051749662));
#34136=CARTESIAN_POINT('Ctrl Pts',(-36.1543446910254,-5.60298974520627,
1.58170072687855));
#34137=CARTESIAN_POINT('Ctrl Pts',(-36.0150860469425,-5.67540281826104,
-1.29810405005511));
#34138=CARTESIAN_POINT('Ctrl Pts',(-35.8758274028596,-4.35831707567691,
-3.86009631254946));
#34139=CARTESIAN_POINT('Ctrl Pts',(-35.7365687587769,-1.97419228604106,
-5.47702803462159));
#34140=CARTESIAN_POINT('Ctrl Pts',(-35.597310114694,0.893270502876724,-5.75302868782914));
#34141=CARTESIAN_POINT('Ctrl Pts',(-35.4580514706112,3.54203545737847,-4.62052552129825));
#34142=CARTESIAN_POINT('Ctrl Pts',(-35.3187928265283,5.32361014705135,-2.35678727858641));
#34143=CARTESIAN_POINT('Ctrl Pts',(-35.1795341824455,5.80181479742939,0.483959017504846));
#34144=CARTESIAN_POINT('Ctrl Pts',(-35.0402755383626,4.85957141130056,3.20621848487671));
#34145=CARTESIAN_POINT('Ctrl Pts',(-34.9010168942798,2.72756776731154,5.14350516175671));
#34146=CARTESIAN_POINT('Ctrl Pts',(-34.7617582501969,-0.0722214601182912,
5.82151658376003));
#34147=CARTESIAN_POINT('Ctrl Pts',(-34.6224996061141,-2.85432883543797,
5.07425641581919));
#34148=CARTESIAN_POINT('Ctrl Pts',(-34.4832409620313,-4.93761593961783,
3.08467504076633));
#34149=CARTESIAN_POINT('Ctrl Pts',(-34.3439823179484,-5.81203528235817,
0.339878141277983));
#34150=CARTESIAN_POINT('Ctrl Pts',(-34.2047236738656,-5.26350432537642,
-2.48813052130279));
#34151=CARTESIAN_POINT('Ctrl Pts',(-34.0654650297828,-3.42631893091784,
-4.70697459711955));
#34152=CARTESIAN_POINT('Ctrl Pts',(-33.9262063856999,-0.750273943763396,
-5.77341842270285));
#34153=CARTESIAN_POINT('Ctrl Pts',(-33.7869477416171,2.10945928361774,-5.42636644588749));
#34154=CARTESIAN_POINT('Ctrl Pts',(-33.6476890975342,4.45273733238242,-3.75078678720913));
#34155=CARTESIAN_POINT('Ctrl Pts',(-33.5084304534514,5.70585958995129,-1.15690864550998));
#34156=CARTESIAN_POINT('Ctrl Pts',(-33.3691718093686,5.56202635443529,1.72021338992062));
#34157=CARTESIAN_POINT('Ctrl Pts',(-33.2299131652857,4.05645206202488,4.17617862917631));
#34158=CARTESIAN_POINT('Ctrl Pts',(-33.0906545212029,1.55774379897477,5.60969745450237));
#34159=CARTESIAN_POINT('Ctrl Pts',(-32.95139587712,-1.32234411818198,5.669803991974));
#34160=CARTESIAN_POINT('Ctrl Pts',(-32.8121372330372,-3.87868486797135,
4.34178246452594));
#34161=CARTESIAN_POINT('Ctrl Pts',(-32.6728785889544,-5.48541407425198,
1.95077002957627));
#34162=CARTESIAN_POINT('Ctrl Pts',(-32.5336199448715,-5.74915907244476,
-0.917845975107423));
#34163=CARTESIAN_POINT('Ctrl Pts',(-32.3943613007887,-4.60534764197699,
-3.5617473760546));
#34164=CARTESIAN_POINT('Ctrl Pts',(-32.2551026567059,-2.33401710862849,
-5.33363247805137));
#34165=CARTESIAN_POINT('Ctrl Pts',(-32.115844012623,0.508746697735507,-5.79969379121329));
#34166=CARTESIAN_POINT('Ctrl Pts',(-31.9765853685402,3.226954951551,-4.84582635006201));
#34167=CARTESIAN_POINT('Ctrl Pts',(-31.8373267244573,5.15511354248211,-2.70556383003843));
#34168=CARTESIAN_POINT('Ctrl Pts',(-31.6980680803746,5.82115481925269,0.0970970884525876));
#34169=CARTESIAN_POINT('Ctrl Pts',(-31.5588094362917,5.06201307624238,2.87598589882601));
#34170=CARTESIAN_POINT('Ctrl Pts',(-31.4195507922089,3.06354764125445,4.95075217760485));
#34171=CARTESIAN_POINT('Ctrl Pts',(-31.280292148126,0.31503926561749,5.81343457307417));
#34172=CARTESIAN_POINT('Ctrl Pts',(-31.1410335040432,-2.51059961519641,
5.25282408295484));
#34173=CARTESIAN_POINT('Ctrl Pts',(-31.0017748599603,-4.7215728408018,3.40617398018623));
#34174=CARTESIAN_POINT('Ctrl Pts',(-30.8625162158775,-5.77657175403985,
0.725596337314116));
#34175=CARTESIAN_POINT('Ctrl Pts',(-30.7232575717947,-5.4173028403555,-2.13262777112443));
#34176=CARTESIAN_POINT('Ctrl Pts',(-30.5839989277118,-3.7317252712905,-4.46872440120295));
#34177=CARTESIAN_POINT('Ctrl Pts',(-30.444740283629,-1.13251601637163,-5.71075115435407));
#34178=CARTESIAN_POINT('Ctrl Pts',(-30.3054816395461,1.7439651281085,-5.55462482137511));
#34179=CARTESIAN_POINT('Ctrl Pts',(-30.1662229954633,4.19347438043934,-4.03856953572594));
#34180=CARTESIAN_POINT('Ctrl Pts',(-30.0269643513805,5.61630273070555,-1.53375842666445));
#34181=CARTESIAN_POINT('Ctrl Pts',(-29.8877057072976,5.6641016350485,1.3465600403011));
#34182=CARTESIAN_POINT('Ctrl Pts',(-29.7484470632148,4.32516857241371,3.89720259859551));
#34183=CARTESIAN_POINT('Ctrl Pts',(-29.609188419132,1.92731215204464,5.49369995020442));
#34184=CARTESIAN_POINT('Ctrl Pts',(-29.4699297750491,-0.942404687467824,
5.74518447739786));
#34185=CARTESIAN_POINT('Ctrl Pts',(-29.3306711309663,-3.58139425721263,
4.59008566899347));
#34186=CARTESIAN_POINT('Ctrl Pts',(-29.1914124868835,-5.34355741690579,
2.31120431951092));
#34187=CARTESIAN_POINT('Ctrl Pts',(-29.0521538428006,-5.79746688257059,
-0.533525088249863));
#34188=CARTESIAN_POINT('Ctrl Pts',(-28.9128951987178,-4.83199280401928,
-3.24763249401785));
#34189=CARTESIAN_POINT('Ctrl Pts',(-28.7736365546349,-2.68351048916141,
-5.16662779081825));
#34190=CARTESIAN_POINT('Ctrl Pts',(-28.6343779105521,0.121970943793783,
-5.8206867604403));
#34191=CARTESIAN_POINT('Ctrl Pts',(-28.4951192664693,2.8975904467026,-5.0496773042911));
#34192=CARTESIAN_POINT('Ctrl Pts',(-28.3558606223864,4.96379801484174,-3.04236430135316));
#34193=CARTESIAN_POINT('Ctrl Pts',(-28.2166019783036,5.81472771045681,-0.290194637339041));
#34194=CARTESIAN_POINT('Ctrl Pts',(-28.0773433342207,5.24204792394922,2.5330228655333));
#34195=CARTESIAN_POINT('Ctrl Pts',(-27.9380846901379,3.38596683270716,4.73608486854933));
#34196=CARTESIAN_POINT('Ctrl Pts',(-27.7988260460551,0.700905481473475,
5.77961960515874));
#34197=CARTESIAN_POINT('Ctrl Pts',(-27.6595674019722,-2.15575731684136,
5.40814031485682));
#34198=CARTESIAN_POINT('Ctrl Pts',(-27.5203087578894,-4.48462987110196,
3.71259561405692));
#34199=CARTESIAN_POINT('Ctrl Pts',(-27.3810501138066,-5.71553844042309,
1.10810270748739));
#34200=CARTESIAN_POINT('Ctrl Pts',(-27.2417914697237,-5.54712186084846,
-1.76768502148767));
#34201=CARTESIAN_POINT('Ctrl Pts',(-27.1025328256409,-4.02061326513478,
-4.21069355884716));
#34202=CARTESIAN_POINT('Ctrl Pts',(-26.9632741815581,-1.50974504792053,
-5.62280545320343));
#34203=CARTESIAN_POINT('Ctrl Pts',(-26.8240155374752,1.37075137422973,-5.65829585160959));
#34204=CARTESIAN_POINT('Ctrl Pts',(-26.6847568933924,3.91564916628817,-4.30847570270991));
#34205=CARTESIAN_POINT('Ctrl Pts',(-26.5454982493095,5.50188551117867,-1.90381908178716));
#34206=CARTESIAN_POINT('Ctrl Pts',(-26.4062396052267,5.74110497526461,0.966946191515625));
#34207=CARTESIAN_POINT('Ctrl Pts',(-26.2669809611438,4.57473988103147,3.60097574210031));
#34208=CARTESIAN_POINT('Ctrl Pts',(-26.1277223170611,2.28834932779543,5.35338478238516));
#34209=CARTESIAN_POINT('Ctrl Pts',(-25.9884636729782,-0.55829373659443,
5.79513411216466));
#34210=CARTESIAN_POINT('Ctrl Pts',(-25.8492050288954,-3.26825073470533,
4.81807102577296));
#34211=CARTESIAN_POINT('Ctrl Pts',(-25.7099463848125,-5.17804769651491,
2.66140814737449));
#34212=CARTESIAN_POINT('Ctrl Pts',(-25.5706877407297,-5.82011241586959,
-0.146842571945131));
#34213=CARTESIAN_POINT('Ctrl Pts',(-25.4314290966468,-5.03724932521661,
-2.91914208456862));
#34214=CARTESIAN_POINT('Ctrl Pts',(-25.292170452564,-3.02112540787031,-4.97675321311146));
#34215=CARTESIAN_POINT('Ctrl Pts',(-25.1529118084812,-0.265344710105641,
-5.81591467089345));
#34216=CARTESIAN_POINT('Ctrl Pts',(-25.0136531643983,2.55539986286478,-5.23117604513226));
#34217=CARTESIAN_POINT('Ctrl Pts',(-24.8743945203155,4.75051041537242,-3.36569785746327));
#34218=CARTESIAN_POINT('Ctrl Pts',(-24.7351358762326,5.7825619204057,-0.676201827096679));
#34219=CARTESIAN_POINT('Ctrl Pts',(-24.5958772321498,5.39887903669928,2.17884749842298));
#34220=CARTESIAN_POINT('Ctrl Pts',(-24.456618588067,3.69339816481585,4.50045345164571));
#34221=CARTESIAN_POINT('Ctrl Pts',(-24.3173599439842,1.0836691646442,5.72022136074243));
#34222=CARTESIAN_POINT('Ctrl Pts',(-24.1781012999013,-1.79137263693289,
5.53951760985943));
#34223=CARTESIAN_POINT('Ctrl Pts',(-24.0388426558185,-4.22783584997752,
4.00258357813294));
#34224=CARTESIAN_POINT('Ctrl Pts',(-23.8995840117356,-5.6292055032563,1.48570410122738));
#34225=CARTESIAN_POINT('Ctrl Pts',(-23.7603253676528,-5.65238674767088,
-1.39491767823394));
#34226=CARTESIAN_POINT('Ctrl Pts',(-23.6210667235699,-4.29170416022648,
-3.93402423421483));
#34227=CARTESIAN_POINT('Ctrl Pts',(-23.4818080794871,-1.88029124778742,
-5.50997060770642));
#34228=CARTESIAN_POINT('Ctrl Pts',(-23.3425494354043,0.991470039123001,
-5.73692064053673));
#34229=CARTESIAN_POINT('Ctrl Pts',(-23.2032907913214,3.62049147315989,-4.55931055830499));
#34230=CARTESIAN_POINT('Ctrl Pts',(-23.0640321472386,5.36311439504185,-2.26545255081397));
#34231=CARTESIAN_POINT('Ctrl Pts',(-22.9247735031558,5.79269552259183,0.583052190493658));
#34232=CARTESIAN_POINT('Ctrl Pts',(-22.7855148590729,4.80406126953481,3.28880929712418));
#34233=CARTESIAN_POINT('Ctrl Pts',(-22.6462562149901,2.63925720826662,5.18937305104455));
#34234=CARTESIAN_POINT('Ctrl Pts',(-22.5069975709072,-0.171711518750607,
5.81943179602813));
#34235=CARTESIAN_POINT('Ctrl Pts',(-22.3677389268244,-2.94064041889114,
5.02472936595383));
#34236=CARTESIAN_POINT('Ctrl Pts',(-22.2284802827415,-4.98961753585213,
2.99983134862808));
#34237=CARTESIAN_POINT('Ctrl Pts',(-22.0892216386588,-5.81699543271016,
0.240489937676924));
#34238=CARTESIAN_POINT('Ctrl Pts',(-21.9499629945759,-5.22020864502445,
-2.57773019858685));
#34239=CARTESIAN_POINT('Ctrl Pts',(-21.8107043504931,-3.34536742456608,
-4.7648492178606));
#34240=CARTESIAN_POINT('Ctrl Pts',(-21.6714457064102,-0.651485825272392,
-5.78539864605405));
#34241=CARTESIAN_POINT('Ctrl Pts',(-21.5321870623274,2.20189789424249,-5.38951917499377));
#34242=CARTESIAN_POINT('Ctrl Pts',(-21.3929284182446,4.51619485389539,-3.67413327411291));
#34243=CARTESIAN_POINT('Ctrl Pts',(-21.2536697741617,5.72479982980199,-1.0592158339988));
#34244=CARTESIAN_POINT('Ctrl Pts',(-21.1144111300789,5.53181220726169,1.81502754190821));
#34245=CARTESIAN_POINT('Ctrl Pts',(-20.975152485996,3.98448080394246,4.24490094081229));
#34246=CARTESIAN_POINT('Ctrl Pts',(-20.8358938419132,1.46163602557251,5.63550276399928));
#34247=CARTESIAN_POINT('Ctrl Pts',(-20.6966351978304,-1.41905851103717,
5.64637443113256));
#34248=CARTESIAN_POINT('Ctrl Pts',(-20.5573765537475,-3.95232746684679,
4.27485425121175));
#34249=CARTESIAN_POINT('Ctrl Pts',(-20.4181179096647,-5.51795509215379,
1.85672907966367));
#34250=CARTESIAN_POINT('Ctrl Pts',(-20.2788592655818,-5.73263154962014,
-1.01597578248433));
#34251=CARTESIAN_POINT('Ctrl Pts',(-20.139600621499,-4.54379798255362,-3.6399410940339));
#34252=CARTESIAN_POINT('Ctrl Pts',(-20.0003419774162,-2.24251440666192,
-5.37274607721308));
#34253=CARTESIAN_POINT('Ctrl Pts',(-19.8610833333333,0.607799997858133,
-5.79015115838078));
#34254=CARTESIAN_POINT('Ctrl Pts',(-19.7218246892505,3.30930780587516,-4.78996379112292));
#34255=CARTESIAN_POINT('Ctrl Pts',(-19.5825660451677,5.20060364760623,-2.61705807631385));
#34256=CARTESIAN_POINT('Ctrl Pts',(-19.4433074010848,5.81864491334401,0.196577330103327));
#34257=CARTESIAN_POINT('Ctrl Pts',(-19.304048757002,5.01211765511721,2.96208505711049));
#34258=CARTESIAN_POINT('Ctrl Pts',(-19.1647901129191,2.97848251245621,5.00239074816106));
#34259=CARTESIAN_POINT('Ctrl Pts',(-19.0255314688363,0.215630773901309,
5.81796997617222));
#34260=CARTESIAN_POINT('Ctrl Pts',(-18.8862728247535,-2.60001346494751,
5.20914592389064));
#34261=CARTESIAN_POINT('Ctrl Pts',(-18.7470141806706,-4.77910101418741,
3.32497590524923));
#34262=CARTESIAN_POINT('Ctrl Pts',(-18.6077555365878,-5.7881297303052,0.62675792731469));
#34263=CARTESIAN_POINT('Ctrl Pts',(-18.468496892505,-5.38006090065132,-2.22490808339976));
#34264=CARTESIAN_POINT('Ctrl Pts',(-18.3292382484221,-3.65480129372495,
-4.53185379041305));
#34265=CARTESIAN_POINT('Ctrl Pts',(-18.1899796043393,-1.034743162069,-5.7292737639989));
#34266=CARTESIAN_POINT('Ctrl Pts',(-18.0507209602564,1.83864930447494,-5.52400579375589));
#34267=CARTESIAN_POINT('Ctrl Pts',(-17.9114623161736,4.26188851974257,-3.96630527312024));
#34268=CARTESIAN_POINT('Ctrl Pts',(-17.7722036720908,5.64169712044425,-1.4375412604395));
#34269=CARTESIAN_POINT('Ctrl Pts',(-17.6329450280079,5.64025901177969,1.44317343182744));
#34270=CARTESIAN_POINT('Ctrl Pts',(-17.4936863839251,4.25792628334514,3.97055852996697));
#34271=CARTESIAN_POINT('Ctrl Pts',(-17.3544277398422,1.83313300766102,5.52583881872415));
#34272=CARTESIAN_POINT('Ctrl Pts',(-17.2151690957594,-1.04046297412495,
5.72823778083364));
#34273=CARTESIAN_POINT('Ctrl Pts',(-17.0759104516766,-3.6593242495723,4.52820243703688));
#34274=CARTESIAN_POINT('Ctrl Pts',(-16.9366518075938,-5.38227965302423,
2.21953531418989));
#34275=CARTESIAN_POINT('Ctrl Pts',(-16.7973931635109,-5.78750106599166,
-0.632536706792661));
#34276=CARTESIAN_POINT('Ctrl Pts',(-16.6581345194281,-4.77577884795741,
-3.32974588665524));
#34277=CARTESIAN_POINT('Ctrl Pts',(-16.5188758753453,-2.59481115687255,
-5.21173928112917));
#34278=CARTESIAN_POINT('Ctrl Pts',(-16.3796172312624,0.221439551953394,
-5.81775178218575));
#34279=CARTESIAN_POINT('Ctrl Pts',(-16.2403585871796,2.98347560764755,-4.99941442299663));
#34280=CARTESIAN_POINT('Ctrl Pts',(-16.1010999430967,5.01507261679947,-2.95707928918434));
#34281=CARTESIAN_POINT('Ctrl Pts',(-15.9618412990139,5.81883828348449,-0.190767672706986));
#34282=CARTESIAN_POINT('Ctrl Pts',(-15.822582654931,5.19798808373605,2.62224925505428));
#34283=CARTESIAN_POINT('Ctrl Pts',(-15.6833240108482,3.3045236718621,4.79326554411477));
#34284=CARTESIAN_POINT('Ctrl Pts',(-15.5440653667654,0.602018584755516,
5.79075512328952));
#34285=CARTESIAN_POINT('Ctrl Pts',(-15.4048067226825,-2.24787764572838,
5.37050438638023));
#34286=CARTESIAN_POINT('Ctrl Pts',(-15.2655480785997,-4.54742997526647,
3.63540257665405));
#34287=CARTESIAN_POINT('Ctrl Pts',(-15.1262894345169,-5.73364308163917,
1.01025159572568));
#34288=CARTESIAN_POINT('Ctrl Pts',(-14.987030790434,-5.5160985118871,-1.86223749329987));
#34289=CARTESIAN_POINT('Ctrl Pts',(-14.8477721463512,-3.94805731755129,
-4.27879827657537));
#34290=CARTESIAN_POINT('Ctrl Pts',(-14.7085135022684,-1.41342024579856,
-5.64778845948229));
#34291=CARTESIAN_POINT('Ctrl Pts',(-14.5692548581855,1.46726200026636,-5.63404060127978));
#34292=CARTESIAN_POINT('Ctrl Pts',(-14.4299962141027,3.98871709067603,-4.24092056573142));
#34293=CARTESIAN_POINT('Ctrl Pts',(-14.2907375700198,5.53362164346046,-1.80950346264411));
#34294=CARTESIAN_POINT('Ctrl Pts',(-14.151478925937,5.72373941440754,1.06493116690821));
#34295=CARTESIAN_POINT('Ctrl Pts',(-14.0122202818542,4.51252420652974,3.67864058583845));
#34296=CARTESIAN_POINT('Ctrl Pts',(-13.8729616377713,2.19651569299616,5.39171494839225));
#34297=CARTESIAN_POINT('Ctrl Pts',(-13.7337029936885,-0.65726186560512,
5.78474529381513));
#34298=CARTESIAN_POINT('Ctrl Pts',(-13.5944443496056,-3.3501231662653,4.76150669905519));
#34299=CARTESIAN_POINT('Ctrl Pts',(-13.4551857055228,-5.22277974827667,
2.57251685617135));
#34300=CARTESIAN_POINT('Ctrl Pts',(-13.31592706144,-5.81675241886189,-0.246297730316495));
#34301=CARTESIAN_POINT('Ctrl Pts',(-13.1766684173571,-4.98661990155326,
-3.00481167991068));
#34302=CARTESIAN_POINT('Ctrl Pts',(-13.0374097732743,-2.93562206963557,
-5.02766291019628));
#34303=CARTESIAN_POINT('Ctrl Pts',(-12.8981511291915,-0.165901088094421,
-5.81960033879168));
#34304=CARTESIAN_POINT('Ctrl Pts',(-12.7588924851086,2.64443716288153,-5.18673532830294));
#34305=CARTESIAN_POINT('Ctrl Pts',(-12.6196338410258,4.80734254899847,-3.28401109786243));
#34306=CARTESIAN_POINT('Ctrl Pts',(-12.480375196943,5.79327477706733,-0.577268249335009));
#34307=CARTESIAN_POINT('Ctrl Pts',(-12.3411165528601,5.36084980668236,2.27080616180433));
#34308=CARTESIAN_POINT('Ctrl Pts',(-12.2018579087773,3.61593747712075,4.56292312403445));
#34309=CARTESIAN_POINT('Ctrl Pts',(-12.0625992646944,0.985741582185208,
5.73790770293893));
#34310=CARTESIAN_POINT('Ctrl Pts',(-11.9233406206116,-1.8857916776622,5.50809050604244));
#34311=CARTESIAN_POINT('Ctrl Pts',(-11.7840819765287,-4.29562990253827,
3.92973727044363));
#34312=CARTESIAN_POINT('Ctrl Pts',(-11.6448233324459,-5.6537766698856,1.38927342209956));
#34313=CARTESIAN_POINT('Ctrl Pts',(-11.5055646883631,-5.62771931318099,
-1.49132377649678));
#34314=CARTESIAN_POINT('Ctrl Pts',(-11.3663060442803,-4.22383740889487,
-4.00680281739882));
#34315=CARTESIAN_POINT('Ctrl Pts',(-11.2270474001974,-1.7858408760882,-5.54130342424841));
#34316=CARTESIAN_POINT('Ctrl Pts',(-11.0877887561146,1.08937991404511,-5.71913653248196));
#34317=CARTESIAN_POINT('Ctrl Pts',(-10.9485301120317,3.69788975011609,-4.49676357731658));
#34318=CARTESIAN_POINT('Ctrl Pts',(-10.8092714679489,5.40105179102856,-2.1734559634191));
#34319=CARTESIAN_POINT('Ctrl Pts',(-10.6700128238661,5.78188389217159,0.681975022813711));
#34320=CARTESIAN_POINT('Ctrl Pts',(-10.5307541797832,4.74714760502601,3.37043927261576));
#34321=CARTESIAN_POINT('Ctrl Pts',(-10.3914955357004,2.55017558130455,5.23372484744972));
#34322=CARTESIAN_POINT('Ctrl Pts',(-10.2522368916175,-0.271151411282281,
5.81564684162084));
#34323=CARTESIAN_POINT('Ctrl Pts',(-10.1129782475347,-3.02609288430336,
4.97373432441496));
#34324=CARTESIAN_POINT('Ctrl Pts',(-9.97371960345188,-5.0401613984529,2.91411124561851));
#34325=CARTESIAN_POINT('Ctrl Pts',(-9.83446095936901,-5.82025612817856,
0.141031474127366));
#34326=CARTESIAN_POINT('Ctrl Pts',(-9.69520231528622,-5.17538786306668,
-2.66657678327793));
#34327=CARTESIAN_POINT('Ctrl Pts',(-9.55594367120334,-3.26343855781002,
-4.82133177179226));
#34328=CARTESIAN_POINT('Ctrl Pts',(-9.41668502712053,-0.552507372994592,
-5.79568864562974));
#34329=CARTESIAN_POINT('Ctrl Pts',(-9.27742638303768,2.29369321295268,-5.35109733785042));
#34330=CARTESIAN_POINT('Ctrl Pts',(-9.13816773895486,4.57833295381206,-3.59640635055793));
#34331=CARTESIAN_POINT('Ctrl Pts',(-8.99890909487199,5.74206755002624,-0.961213569000321));
#34332=CARTESIAN_POINT('Ctrl Pts',(-8.85965045078918,5.49998192244803,1.90931142746273));
#34333=CARTESIAN_POINT('Ctrl Pts',(-8.72039180670633,3.91134546632114,4.31238309028591));
#34334=CARTESIAN_POINT('Ctrl Pts',(-8.58113316262349,1.3651012302635,5.65966164230935));
#34335=CARTESIAN_POINT('Ctrl Pts',(-8.44187451854066,-1.51535832115029,
5.62129526291009));
#34336=CARTESIAN_POINT('Ctrl Pts',(-8.30261587445782,-4.02481537988956,
4.20667712477429));
#34337=CARTESIAN_POINT('Ctrl Pts',(-8.16335723037498,-5.54888402081865,
1.76214568007252));
#34338=CARTESIAN_POINT('Ctrl Pts',(-8.02409858629214,-5.71442921910558,
-1.1138087691014));
#34339=CARTESIAN_POINT('Ctrl Pts',(-7.88483994220931,-4.48092083718648,
-3.71707139091558));
#34340=CARTESIAN_POINT('Ctrl Pts',(-7.74558129812645,-2.1503565465292,-5.4102900104425));
#34341=CARTESIAN_POINT('Ctrl Pts',(-7.60632265404363,0.706675727156433,
-5.77891691331019));
#34342=CARTESIAN_POINT('Ctrl Pts',(-7.4670640099608,3.39069383473469,-4.73270182806681));
#34343=CARTESIAN_POINT('Ctrl Pts',(-7.32780536587796,5.24457437879084,-2.52778774022372));
#34344=CARTESIAN_POINT('Ctrl Pts',(-7.18854672179512,5.81443507065043,0.296000141022397));
#34345=CARTESIAN_POINT('Ctrl Pts',(-7.04928807771229,4.96075792687253,3.04731883223044));
#34346=CARTESIAN_POINT('Ctrl Pts',(-6.91002943362943,2.89254720992126,5.05256785334662));
#34347=CARTESIAN_POINT('Ctrl Pts',(-6.77077078954661,0.116159284925314,
5.82080563967053));
#34348=CARTESIAN_POINT('Ctrl Pts',(-6.63151214546377,-2.688667711974,5.16394589523199));
#34349=CARTESIAN_POINT('Ctrl Pts',(-6.49225350138093,-4.83523295705307,
3.24280642735931));
#34350=CARTESIAN_POINT('Ctrl Pts',(-6.35299485729808,-5.79799668489952,
0.527736407867602));
#34351=CARTESIAN_POINT('Ctrl Pts',(-6.21373621321526,-5.34124715796441,
-2.31653838125593));
#34352=CARTESIAN_POINT('Ctrl Pts',(-6.07447756913242,-3.57680955360403,
-4.59365918321567));
#34353=CARTESIAN_POINT('Ctrl Pts',(-5.93521892504958,-0.936668004052796,
-5.74612254694228));
#34354=CARTESIAN_POINT('Ctrl Pts',(-5.79596028096675,1.93279631323058,-5.49177290916668));
#34355=CARTESIAN_POINT('Ctrl Pts',(-5.6567016368839,4.32905753390492,-3.89288224101835));
#34356=CARTESIAN_POINT('Ctrl Pts',(-5.51744299280107,5.66544326929399,-1.34090411167474));
#34357=CARTESIAN_POINT('Ctrl Pts',(-5.37818434871822,5.61476856777023,1.53936519535622));
#34358=CARTESIAN_POINT('Ctrl Pts',(-5.2389257046354,4.18944002671629,4.04275444923907));
#34359=CARTESIAN_POINT('Ctrl Pts',(-5.09966706055255,1.73841830727115,5.55636329474948));
#34360=CARTESIAN_POINT('Ctrl Pts',(-4.96040841646972,-1.13821728600617,
5.70961756023392));
#34361=CARTESIAN_POINT('Ctrl Pts',(-4.82114977238688,-3.73618515797981,
4.46499627542801));
#34362=CARTESIAN_POINT('Ctrl Pts',(-4.68189112830405,-5.419429437944,2.12721786412234));
#34363=CARTESIAN_POINT('Ctrl Pts',(-4.5426324842212,-5.77584441140805,-0.731363527598105));
#34364=CARTESIAN_POINT('Ctrl Pts',(-4.40337384013837,-4.71816963195763,
-3.41088648277354));
#34365=CARTESIAN_POINT('Ctrl Pts',(-4.26411519605553,-2.50535374173064,
-5.25532814418794));
#34366=CARTESIAN_POINT('Ctrl Pts',(-4.12485655197268,0.320843465798982,
-5.81311712807697));
#34367=CARTESIAN_POINT('Ctrl Pts',(-3.98559790788985,3.06848913610684,-4.94769094587604));
#34368=CARTESIAN_POINT('Ctrl Pts',(-3.84633926380702,5.06488204833466,-2.87093035630064));
#34369=CARTESIAN_POINT('Ctrl Pts',(-3.70708061972418,5.82124886323545,-0.0912849746588416));
#34370=CARTESIAN_POINT('Ctrl Pts',(-3.56782197564134,5.1524096337254,2.71070954559799));
#34371=CARTESIAN_POINT('Ctrl Pts',(-3.42856333155851,3.22211508326084,4.84904585092794));
#34372=CARTESIAN_POINT('Ctrl Pts',(-3.28930468747566,0.50295580625768,5.80019885276506));
#34373=CARTESIAN_POINT('Ctrl Pts',(-3.15004604339282,-2.3393412495323,5.33129944682399));
#34374=CARTESIAN_POINT('Ctrl Pts',(-3.01078739931,-4.60890153244437,3.55714744422309));
#34375=CARTESIAN_POINT('Ctrl Pts',(-2.87152875522714,-5.7500726195336,0.912105335297638));
#34376=CARTESIAN_POINT('Ctrl Pts',(-2.73227011114431,-5.48346361630806,
-1.95624590565041));
#34377=CARTESIAN_POINT('Ctrl Pts',(-2.59301146706147,-3.87434793125781,
-4.34565292985953));
#34378=CARTESIAN_POINT('Ctrl Pts',(-2.45375282297864,-1.31668250898415,
-5.6711214434338));
#34379=CARTESIAN_POINT('Ctrl Pts',(-2.3144941788958,1.56334396233179,-5.60813935051552));
#34380=CARTESIAN_POINT('Ctrl Pts',(-2.17523553481297,4.06061969479119,-4.17212642249236));
#34381=CARTESIAN_POINT('Ctrl Pts',(-2.03597689073013,5.56374111549523,-1.71465920456093));
#34382=CARTESIAN_POINT('Ctrl Pts',(-1.89671824664728,5.70470163197095,1.16260504562314));
#34383=CARTESIAN_POINT('Ctrl Pts',(-1.75745960256445,4.44899020576231,3.75523065046461));
#34384=CARTESIAN_POINT('Ctrl Pts',(-1.61820095848162,2.10404029395573,5.42847000776503));
#34385=CARTESIAN_POINT('Ctrl Pts',(-1.47894231439877,-0.756037886019822,
5.77266624528129));
#34386=CARTESIAN_POINT('Ctrl Pts',(-1.33968367031594,-3.43101701838151,
4.70355166697811));
#34387=CARTESIAN_POINT('Ctrl Pts',(-1.20042502623311,-5.26598561487944,
2.48287324446187));
#34388=CARTESIAN_POINT('Ctrl Pts',(-1.06116638215026,-5.81169368649649,
-0.345679466703461));
#34389=CARTESIAN_POINT('Ctrl Pts',(-0.921907738067424,-4.9345323547016,
-3.08960626820369));
#34390=CARTESIAN_POINT('Ctrl Pts',(-0.782649093984597,-2.84926354822401,
-5.0770981807467));
#34391=CARTESIAN_POINT('Ctrl Pts',(-0.643390449901746,-0.0664041808042648,
-5.82159667367763));
#34392=CARTESIAN_POINT('Ctrl Pts',(-0.504131805818908,2.73269248345949,
-5.140758053774));
#34393=CARTESIAN_POINT('Ctrl Pts',(-0.364873161736075,4.86278854237602,
-3.20140635770316));
#34394=CARTESIAN_POINT('Ctrl Pts',(-0.225614517653243,5.80225927534941,
-0.478084902857893));
#34395=CARTESIAN_POINT('Ctrl Pts',(-0.0863558735703991,5.32132481240374,
2.36194063957689));
#34396=CARTESIAN_POINT('Ctrl Pts',(0.0529027705124292,3.53727759009006,
4.62439958704637));
#34397=CARTESIAN_POINT('Ctrl Pts',(0.145741866567655,1.77099953538148,5.37678124514415));
#34398=CARTESIAN_POINT('Ctrl Pts',(0.192161414595269,0.851236939700787,
5.51865210108108));
#34399=CARTESIAN_POINT('Ctrl Pts',(-59.7754114145953,3.05041111877658,-4.27420965560363));
#34400=CARTESIAN_POINT('Ctrl Pts',(-59.7289918665677,3.76276951631921,-3.76581485246873));
#34401=CARTESIAN_POINT('Ctrl Pts',(-59.6361527705124,4.92764081706816,-2.38646903685034));
#34402=CARTESIAN_POINT('Ctrl Pts',(-59.4968941264296,5.46835202429936,0.268532173657807));
#34403=CARTESIAN_POINT('Ctrl Pts',(-59.3576354823467,4.67030006375477,2.85707072904638));
#34404=CARTESIAN_POINT('Ctrl Pts',(-59.2183768382639,2.7288083410323,4.74647128728181));
#34405=CARTESIAN_POINT('Ctrl Pts',(-59.0791181941811,0.119236398296101,
5.47362186748481));
#34406=CARTESIAN_POINT('Ctrl Pts',(-58.9398595500982,-2.5195326040976,4.86076733852051));
#34407=CARTESIAN_POINT('Ctrl Pts',(-58.8006009060154,-4.54144653710774,
3.05781259658032));
#34408=CARTESIAN_POINT('Ctrl Pts',(-58.6613422619325,-5.4514873740282,0.506243184157782));
#34409=CARTESIAN_POINT('Ctrl Pts',(-58.5220836178498,-5.02684959533072,
-2.16928123765479));
#34410=CARTESIAN_POINT('Ctrl Pts',(-58.3828249737669,-3.37149745588529,
-4.3136980286988));
#34411=CARTESIAN_POINT('Ctrl Pts',(-58.2435663296841,-0.890707405090836,
-5.40200302908979));
#34412=CARTESIAN_POINT('Ctrl Pts',(-58.1043076856012,1.80815287776022,-5.16774353188138));
#34413=CARTESIAN_POINT('Ctrl Pts',(-57.9650490415184,4.06432633833454,-3.6682753974527));
#34414=CARTESIAN_POINT('Ctrl Pts',(-57.8257903974356,5.32543796117294,-1.27070945920114));
#34415=CARTESIAN_POINT('Ctrl Pts',(-57.6865317533527,5.2827320554894,1.43796179978132));
#34416=CARTESIAN_POINT('Ctrl Pts',(-57.5472731092699,3.94666421546139,3.79457953437703));
#34417=CARTESIAN_POINT('Ctrl Pts',(-57.4080144651871,1.64434157169202,5.22217702626599));
#34418=CARTESIAN_POINT('Ctrl Pts',(-57.2687558211042,-1.06056230695092,
5.37123820032749));
#34419=CARTESIAN_POINT('Ctrl Pts',(-57.1294971770214,-3.50581059443648,
4.20526862770603));
#34420=CARTESIAN_POINT('Ctrl Pts',(-56.9902385329385,-5.09273748649819,
2.0097305963032));
#34421=CARTESIAN_POINT('Ctrl Pts',(-56.8509798888557,-5.43281848345632,
-0.677846219983215));
#34422=CARTESIAN_POINT('Ctrl Pts',(-56.7117212447728,-4.4427921577306,-3.19946714523332));
#34423=CARTESIAN_POINT('Ctrl Pts',(-56.5724626006901,-2.36504490024336,
-4.93776819958314));
#34424=CARTESIAN_POINT('Ctrl Pts',(-56.4332039566072,0.291732109474193,
-5.46716421440776));
#34425=CARTESIAN_POINT('Ctrl Pts',(-56.2939453125243,2.87708486376904,-4.65804410227385));
#34426=CARTESIAN_POINT('Ctrl Pts',(-56.1546866684415,4.75804602882236,-2.70850330611462));
#34427=CARTESIAN_POINT('Ctrl Pts',(-56.0154280243586,5.47410321551656,-0.0958444448425244));
#34428=CARTESIAN_POINT('Ctrl Pts',(-55.8761693802759,4.84994541162324,2.54027984206958));
#34429=CARTESIAN_POINT('Ctrl Pts',(-55.7369107361929,3.03838406631521,4.55447191639935));
#34430=CARTESIAN_POINT('Ctrl Pts',(-55.5976520921102,0.482940533822174,
5.45360070160385));
#34431=CARTESIAN_POINT('Ctrl Pts',(-55.4583934480273,-2.19074047383461,
5.01753409037006));
#34432=CARTESIAN_POINT('Ctrl Pts',(-55.3191348039445,-4.32806637309799,
3.35303349845926));
#34433=CARTESIAN_POINT('Ctrl Pts',(-55.1798761598616,-5.40575945122019,
0.867615656424194));
#34434=CARTESIAN_POINT('Ctrl Pts',(-55.0406175157789,-5.15997002146987,
-1.83021898942756));
#34435=CARTESIAN_POINT('Ctrl Pts',(-54.9013588716959,-3.65087427441368,
-4.07996436309852));
#34436=CARTESIAN_POINT('Ctrl Pts',(-54.7621002276132,-1.24794144780751,
-5.33081929111963));
#34437=CARTESIAN_POINT('Ctrl Pts',(-54.6228415835303,1.46052267221381,-5.27653917787774));
#34438=CARTESIAN_POINT('Ctrl Pts',(-54.4835829394475,3.81140961432537,-3.9304133273178));
#34439=CARTESIAN_POINT('Ctrl Pts',(-54.3443242953646,5.22915589407203,-1.622011346206));
#34440=CARTESIAN_POINT('Ctrl Pts',(-54.2050656512818,5.36665720191545,1.08350479872415));
#34441=CARTESIAN_POINT('Ctrl Pts',(-54.0658070071989,4.19024933629756,3.52374838366578));
#34442=CARTESIAN_POINT('Ctrl Pts',(-53.9265483631161,1.98795015045772,5.10127889563238));
#34443=CARTESIAN_POINT('Ctrl Pts',(-53.7872897190333,-0.701055348231372,
5.42987233463601));
#34444=CARTESIAN_POINT('Ctrl Pts',(-53.6480310749504,-3.2184227082265,4.42907975124644));
#34445=CARTESIAN_POINT('Ctrl Pts',(-53.5087724308676,-4.94782933935193,
2.34392342033126));
#34446=CARTESIAN_POINT('Ctrl Pts',(-53.3695137867847,-5.46586768047832,
-0.315091528340425));
#34447=CARTESIAN_POINT('Ctrl Pts',(-53.2302551427019,-4.64570732246977,
-2.8969631764453));
#34448=CARTESIAN_POINT('Ctrl Pts',(-53.0909964986191,-2.68814667251956,
-4.76957646324611));
#34449=CARTESIAN_POINT('Ctrl Pts',(-52.9517378545362,-0.0724518359154483,
-5.47446279585511));
#34450=CARTESIAN_POINT('Ctrl Pts',(-52.8124792104534,2.56098125529703,-4.83904610246136));
#34451=CARTESIAN_POINT('Ctrl Pts',(-52.6732205663706,4.56741384362734,-3.01889432620133));
#34452=CARTESIAN_POINT('Ctrl Pts',(-52.5339619222877,5.45561459371124,-0.459632001294636));
#34453=CARTESIAN_POINT('Ctrl Pts',(-52.3947032782049,5.00812688972579,2.21216121205818));
#34454=CARTESIAN_POINT('Ctrl Pts',(-52.2554446341221,3.33450835332562,4.34235491563401));
#34455=CARTESIAN_POINT('Ctrl Pts',(-52.1161859900392,0.844508045260551,
5.4094175595178));
#34456=CARTESIAN_POINT('Ctrl Pts',(-51.9769273459563,-1.85225167112555,
5.15210208735637));
#34457=CARTESIAN_POINT('Ctrl Pts',(-51.8376687018735,-4.09552789291051,
3.63340659025675));
#34458=CARTESIAN_POINT('Ctrl Pts',(-51.6984100577907,-5.33610327761922,
1.22515059576798));
#34459=CARTESIAN_POINT('Ctrl Pts',(-51.5591514137078,-5.27024995201298,
-1.48305684821466));
#34460=CARTESIAN_POINT('Ctrl Pts',(-51.419892769625,-3.91409066911317,-3.828170111906));
#34461=CARTESIAN_POINT('Ctrl Pts',(-51.2806341255422,-1.5996515031473,-5.23603927030803));
#34462=CARTESIAN_POINT('Ctrl Pts',(-51.1413754814594,1.1064275058807,-5.36197821199973));
#34463=CARTESIAN_POINT('Ctrl Pts',(-51.0021168373765,3.54162182914421,-4.1751535290404));
#34464=CARTESIAN_POINT('Ctrl Pts',(-50.8628581932937,5.10972715544653,-1.96613340560134));
#34465=CARTESIAN_POINT('Ctrl Pts',(-50.7235995492108,5.42682703630521,0.724251675701316));
#34466=CARTESIAN_POINT('Ctrl Pts',(-50.584340905128,4.41528646976498,3.23731950255755));
#34467=CARTESIAN_POINT('Ctrl Pts',(-50.4450822610451,2.32275914036367,4.95780013187161));
#34468=CARTESIAN_POINT('Ctrl Pts',(-50.3058236169624,-0.338445193631064,
5.46447133972146));
#34469=CARTESIAN_POINT('Ctrl Pts',(-50.1665649728795,-2.91678859056669,
4.6332857120697));
#34470=CARTESIAN_POINT('Ctrl Pts',(-50.0273063287967,-4.78101980518796,
2.66774095334042));
#34471=CARTESIAN_POINT('Ctrl Pts',(-49.8880476847138,-5.47472241248648,
0.0490579040265954));
#34472=CARTESIAN_POINT('Ctrl Pts',(-49.7487890406309,-4.8280584323024,-2.58163590500342));
#34473=CARTESIAN_POINT('Ctrl Pts',(-49.6095303965482,-2.99934946106781,
-4.58027236986203));
#34474=CARTESIAN_POINT('Ctrl Pts',(-49.4702717524653,-0.436315075885255,
-5.45752886628046));
#34475=CARTESIAN_POINT('Ctrl Pts',(-49.3310131083825,2.23354155621114,-4.99862824066834));
#34476=CARTESIAN_POINT('Ctrl Pts',(-49.1917544642996,4.35656416675584,-3.31592232005941));
#34477=CARTESIAN_POINT('Ctrl Pts',(-49.0524958202167,5.41297689183398,-0.821385013377194));
#34478=CARTESIAN_POINT('Ctrl Pts',(-48.913237176134,5.14414007584278,1.87425053070219));
#34479=CARTESIAN_POINT('Ctrl Pts',(-48.773978532051,3.61587256008425,4.11101663837049));
#34480=CARTESIAN_POINT('Ctrl Pts',(-48.6347198879684,1.20233737247478,5.34128982685639));
#34481=CARTESIAN_POINT('Ctrl Pts',(-48.4954612438854,-1.50556394359286,
5.26386449136776));
#34482=CARTESIAN_POINT('Ctrl Pts',(-48.3562025998026,-3.84486070708852,
3.89769653960079));
#34483=CARTESIAN_POINT('Ctrl Pts',(-48.2169439557197,-5.2428270364507,1.57726245044722));
#34484=CARTESIAN_POINT('Ctrl Pts',(-48.0776853116369,-5.35720131234524,
-1.12933000966752));
#34485=CARTESIAN_POINT('Ctrl Pts',(-47.9384266675541,-4.15998148346686,
-3.55943060459705));
#34486=CARTESIAN_POINT('Ctrl Pts',(-47.7991680234712,-1.94428075914289,
-5.11808211162696));
#34487=CARTESIAN_POINT('Ctrl Pts',(-47.6599093793885,0.747434778333361,
-5.42368264409589));
#34488=CARTESIAN_POINT('Ctrl Pts',(-47.5206507353055,3.25615718342438,-4.40141256513894));
#34489=CARTESIAN_POINT('Ctrl Pts',(-47.3813920912228,4.96768039494549,-2.30155244680704));
#34490=CARTESIAN_POINT('Ctrl Pts',(-47.2421334471398,5.46297521770101,0.361792678911387));
#34491=CARTESIAN_POINT('Ctrl Pts',(-47.1028748030571,4.62077949785816,2.93656074411938));
#34492=CARTESIAN_POINT('Ctrl Pts',(-46.9636161589742,2.64728652120321,4.79237584569334));
#34493=CARTESIAN_POINT('Ctrl Pts',(-46.8243575148914,0.0256630763402578,
5.47488206066962));
#34494=CARTESIAN_POINT('Ctrl Pts',(-46.6850988708086,-2.60224341403018,
4.81698260178151));
#34495=CARTESIAN_POINT('Ctrl Pts',(-46.5458402267257,-4.59304726030904,
2.97974982780383));
#34496=CARTESIAN_POINT('Ctrl Pts',(-46.4065815826429,-5.45934348435565,
0.41299018336124));
#34497=CARTESIAN_POINT('Ctrl Pts',(-46.26732293856,-4.98903831664372,-2.25488111588837));
#34498=CARTESIAN_POINT('Ctrl Pts',(-46.1280642944772,-3.29727573804136,
-4.37069386700247));
#34499=CARTESIAN_POINT('Ctrl Pts',(-45.9888056503943,-0.798246983000946,
-5.41643738317532));
#34500=CARTESIAN_POINT('Ctrl Pts',(-45.8495470063115,1.89621516645834,-5.13608413231546));
#34501=CARTESIAN_POINT('Ctrl Pts',(-45.7102883622287,4.12643031665392,-3.59827250406756));
#34502=CARTESIAN_POINT('Ctrl Pts',(-45.5710297181459,5.34637884412477,-1.17950219449742));
#34503=CARTESIAN_POINT('Ctrl Pts',(-45.431771074063,5.2573829125406,1.5280435473688));
#34504=CARTESIAN_POINT('Ctrl Pts',(-45.2925124299802,3.8812312381375,3.86148109510261));
#34505=CARTESIAN_POINT('Ctrl Pts',(-45.1532537858974,1.55484459692986,5.24951906855545));
#34506=CARTESIAN_POINT('Ctrl Pts',(-45.0139951418145,-1.1522118918849,5.35232659017816));
#34507=CARTESIAN_POINT('Ctrl Pts',(-44.8747364977316,-3.57717438483602,
4.14473347661853));
#34508=CARTESIAN_POINT('Ctrl Pts',(-44.7354778536489,-5.12634361161217,
1.92239261011174));
#34509=CARTESIAN_POINT('Ctrl Pts',(-44.5962192095659,-5.42043921542468,
-0.770604232804061));
#34510=CARTESIAN_POINT('Ctrl Pts',(-44.4569605654832,-4.38745829070579,
-3.27493540685099));
#34511=CARTESIAN_POINT('Ctrl Pts',(-44.3177019214003,-2.28030372689555,
-4.97746994815997));
#34512=CARTESIAN_POINT('Ctrl Pts',(-44.1784432773175,0.385133557856286,
-5.46137934173613));
#34513=CARTESIAN_POINT('Ctrl Pts',(-44.0391846332346,2.95627927606374,-4.60818890819867));
#34514=CARTESIAN_POINT('Ctrl Pts',(-43.8999259891518,4.8036443774009,-2.62678374960595));
#34515=CARTESIAN_POINT('Ctrl Pts',(-43.7606673450689,5.47494173748935,-0.00226778004610677));
#34516=CARTESIAN_POINT('Ctrl Pts',(-43.6214087009862,4.80581881314338,2.62280340608412));
#34517=CARTESIAN_POINT('Ctrl Pts',(-43.4821500569032,2.96009578429874,4.60573828169883));
#34518=CARTESIAN_POINT('Ctrl Pts',(-43.3428914128205,0.389657749635209,
5.46105841480188));
#34519=CARTESIAN_POINT('Ctrl Pts',(-43.2036327687376,-2.27617950142941,
4.97935729276398));
#34520=CARTESIAN_POINT('Ctrl Pts',(-43.0643741246547,-4.38474375836553,
3.27856894775812));
#34521=CARTESIAN_POINT('Ctrl Pts',(-42.925115480572,-5.41979897035326,0.775094376632309));
#34522=CARTESIAN_POINT('Ctrl Pts',(-42.7858568364891,-5.12793440387594,
-1.91814517731967));
#34523=CARTESIAN_POINT('Ctrl Pts',(-42.6465981924063,-3.58060674358378,
-4.14176864630699));
#34524=CARTESIAN_POINT('Ctrl Pts',(-42.5073395483234,-1.15664547880632,
-5.35137023649888));
#34525=CARTESIAN_POINT('Ctrl Pts',(-42.3680809042406,1.55049524906482,-5.25080533388515));
#34526=CARTESIAN_POINT('Ctrl Pts',(-42.2288222601577,3.87803097245991,-3.86469506537978));
#34527=CARTESIAN_POINT('Ctrl Pts',(-42.0895636160749,5.2561152444257,-1.53239835194539));
#34528=CARTESIAN_POINT('Ctrl Pts',(-41.9503049719921,5.34735413451096,1.17507273470952));
#34529=CARTESIAN_POINT('Ctrl Pts',(-41.8110463279092,4.12940978692406,3.59485284585963));
#34530=CARTESIAN_POINT('Ctrl Pts',(-41.6717876838264,1.90046935818554,5.13451150454715));
#34531=CARTESIAN_POINT('Ctrl Pts',(-41.5325290397435,-0.793759616039144,
5.41709680951658));
#34532=CARTESIAN_POINT('Ctrl Pts',(-41.3932703956607,-3.29365382994698,
4.37342390127059));
#34533=CARTESIAN_POINT('Ctrl Pts',(-41.2540117515779,-4.98716861275776,
2.25901336863089));
#34534=CARTESIAN_POINT('Ctrl Pts',(-41.114753107495,-5.45968374096753,-0.408467404261251));
#34535=CARTESIAN_POINT('Ctrl Pts',(-40.9754944634122,-4.59551417299541,
-2.9759438263394));
#34536=CARTESIAN_POINT('Ctrl Pts',(-40.8362358193294,-2.60623301292921,
-4.81482519454727));
#34537=CARTESIAN_POINT('Ctrl Pts',(-40.6969771752465,0.0211275576577767,
-5.47490144185597));
#34538=CARTESIAN_POINT('Ctrl Pts',(-40.5577185311637,2.64331550573975,-4.7945672702388));
#34539=CARTESIAN_POINT('Ctrl Pts',(-40.4184598870809,4.61834520229331,-2.94038768943546));
#34540=CARTESIAN_POINT('Ctrl Pts',(-40.279201242998,5.46267362630453,-0.366318200757423));
#34541=CARTESIAN_POINT('Ctrl Pts',(-40.1399425989152,4.9695853458046,2.29743632392573));
#34542=CARTESIAN_POINT('Ctrl Pts',(-40.0006839548323,3.25980229079568,4.39871358429398));
#34543=CARTESIAN_POINT('Ctrl Pts',(-39.8614253107496,0.75192761703796,5.42306159198518));
#34544=CARTESIAN_POINT('Ctrl Pts',(-39.7221666666666,-1.94004016284409,
5.11969103933832));
#34545=CARTESIAN_POINT('Ctrl Pts',(-39.5829080225839,-4.15703134725169,
3.56287560120978));
#34546=CARTESIAN_POINT('Ctrl Pts',(-39.443649378501,-5.35626391283587,1.13376764276522));
#34547=CARTESIAN_POINT('Ctrl Pts',(-39.3043907344182,-5.24413187550802,
-1.57291863871278));
#34548=CARTESIAN_POINT('Ctrl Pts',(-39.1651320903353,-3.84808832327816,
-3.89451003695966));
#34549=CARTESIAN_POINT('Ctrl Pts',(-39.0258734462525,-1.50992412536221,
-5.26261544361532));
#34550=CARTESIAN_POINT('Ctrl Pts',(-38.8866148021696,1.19791212070242,-5.34228403614066));
#34551=CARTESIAN_POINT('Ctrl Pts',(-38.7473561580868,3.61246566485912,-4.11401069419408));
#34552=CARTESIAN_POINT('Ctrl Pts',(-38.608097514004,5.14258564128613,-1.87851140368299));
#34553=CARTESIAN_POINT('Ctrl Pts',(-38.4688388699211,5.41365548740393,0.816900505221123));
#34554=CARTESIAN_POINT('Ctrl Pts',(-38.3295802258383,4.35930965310145,3.31231211091373));
#34555=CARTESIAN_POINT('Ctrl Pts',(-38.1903215817555,2.23768176077518,4.99677621164119));
#34556=CARTESIAN_POINT('Ctrl Pts',(-38.0510629376726,-0.43179379205009,
5.45788844635691));
#34557=CARTESIAN_POINT('Ctrl Pts',(-37.9118042935898,-2.99555403587155,
4.58275552368911));
#34558=CARTESIAN_POINT('Ctrl Pts',(-37.7725456495069,-4.82591809297065,
2.58563468642958));
#34559=CARTESIAN_POINT('Ctrl Pts',(-37.6332870054241,-5.4747611745053,-0.0445225095723984));
#34560=CARTESIAN_POINT('Ctrl Pts',(-37.4940283613413,-4.78322817852097,
-2.66377933844605));
#34561=CARTESIAN_POINT('Ctrl Pts',(-37.3547697172584,-2.92062590308386,
-4.63086779189008));
#34562=CARTESIAN_POINT('Ctrl Pts',(-37.2155110731756,-0.342971962908202,
-5.46418908936982));
#34563=CARTESIAN_POINT('Ctrl Pts',(-37.0762524290927,2.3186511952276,-4.95972265420142));
#34564=CARTESIAN_POINT('Ctrl Pts',(-36.9369937850099,4.41260308969872,-3.24097610983336));
#34565=CARTESIAN_POINT('Ctrl Pts',(-36.7977351409271,5.42622518849562,-0.728747127242984));
#34566=CARTESIAN_POINT('Ctrl Pts',(-36.6584764968442,5.11135418922643,1.96189972322917));
#34567=CARTESIAN_POINT('Ctrl Pts',(-36.5192178527614,3.54507940071622,4.17221814079114));
#34568=CARTESIAN_POINT('Ctrl Pts',(-36.3799592086785,1.1108691041234,5.3610597837772));
#34569=CARTESIAN_POINT('Ctrl Pts',(-36.2407005645957,-1.59531330686152,
5.23736265926658));
#34570=CARTESIAN_POINT('Ctrl Pts',(-36.1014419205129,-3.91091798769402,
3.83141131507184));
#34571=CARTESIAN_POINT('Ctrl Pts',(-35.9621832764301,-5.26901954743058,
1.48742232755986));
#34572=CARTESIAN_POINT('Ctrl Pts',(-35.8229246323472,-5.33711638764732,
-1.22072963281623));
#34573=CARTESIAN_POINT('Ctrl Pts',(-35.6836659882644,-4.09853647961605,
-3.63001252022438));
#34574=CARTESIAN_POINT('Ctrl Pts',(-35.5444073441815,-1.85651914755638,
-5.15056587439533));
#34575=CARTESIAN_POINT('Ctrl Pts',(-35.4051487000987,0.840026477797323,
-5.4101153119253));
#34576=CARTESIAN_POINT('Ctrl Pts',(-35.2658900560158,3.33090990905107,-4.34511580392452));
#34577=CARTESIAN_POINT('Ctrl Pts',(-35.1266314119331,5.0062925693755,-2.21630929284359));
#34578=CARTESIAN_POINT('Ctrl Pts',(-34.9873727678502,5.45599349068633,0.455112295282984));
#34579=CARTESIAN_POINT('Ctrl Pts',(-34.8481141237673,4.56991319325272,3.01510954657769));
#34580=CARTESIAN_POINT('Ctrl Pts',(-34.7088554796845,2.56498914623259,4.83692287011466));
#34581=CARTESIAN_POINT('Ctrl Pts',(-34.5695968356017,-0.0679166485057954,
5.47452093799858));
#34582=CARTESIAN_POINT('Ctrl Pts',(-34.4303381915189,-2.68419453053335,
4.77180174504182));
#34583=CARTESIAN_POINT('Ctrl Pts',(-34.291079547436,-4.6433058218266,2.90081078609419));
#34584=CARTESIAN_POINT('Ctrl Pts',(-34.1518209033532,-5.46560477632539,
0.319619462389833));
#34585=CARTESIAN_POINT('Ctrl Pts',(-34.0125622592703,-4.94976939804717,
-2.33982372795152));
#34586=CARTESIAN_POINT('Ctrl Pts',(-33.8733036151875,-3.22209074863717,
-4.42641202095737));
#34587=CARTESIAN_POINT('Ctrl Pts',(-33.7340449711047,-0.705553330523207,
-5.42928970211729));
#34588=CARTESIAN_POINT('Ctrl Pts',(-33.5947863270218,1.98372345931916,-5.1029240057712));
#34589=CARTESIAN_POINT('Ctrl Pts',(-33.455527682939,4.18732874961437,-3.52721846706185));
#34590=CARTESIAN_POINT('Ctrl Pts',(-33.3162690388561,5.36575776175026,-1.08795028100834));
#34591=CARTESIAN_POINT('Ctrl Pts',(-33.1770103947733,5.23049780876673,1.61767884458434));
#34592=CARTESIAN_POINT('Ctrl Pts',(-33.0377517506905,3.814664345283,3.92725452505383));
#34593=CARTESIAN_POINT('Ctrl Pts',(-32.8984931066076,1.46489336942115,5.2753274389326));
#34594=CARTESIAN_POINT('Ctrl Pts',(-32.7592344625248,-1.2435248544032,5.33185128339217));
#34595=CARTESIAN_POINT('Ctrl Pts',(-32.6199758184419,-3.64749309154975,
4.0829874257492));
#34596=CARTESIAN_POINT('Ctrl Pts',(-32.4807171743591,-5.15845205815569,
1.83449299138441));
#34597=CARTESIAN_POINT('Ctrl Pts',(-32.3414585302762,-5.4064763477243,-0.863137111487432));
#34598=CARTESIAN_POINT('Ctrl Pts',(-32.2021998861935,-4.33084261291954,
-3.34944688476314));
#34599=CARTESIAN_POINT('Ctrl Pts',(-32.0629412421106,-2.19489635509741,
-5.01571751219199));
#34600=CARTESIAN_POINT('Ctrl Pts',(-31.9236825980278,0.478422488163947,
-5.45399890855767));
#34601=CARTESIAN_POINT('Ctrl Pts',(-31.7844239539449,3.03461000137415,-4.55698741618728));
#34602=CARTESIAN_POINT('Ctrl Pts',(-31.6451653098621,4.84783932503205,-2.54429676932585));
#34603=CARTESIAN_POINT('Ctrl Pts',(-31.5059066657792,5.47418073672258,0.091309547280987));
#34604=CARTESIAN_POINT('Ctrl Pts',(-31.3666480216964,4.76028817844798,2.7045607092202));
#34605=CARTESIAN_POINT('Ctrl Pts',(-31.2273893776135,2.88094270029059,4.65565906498442));
#34606=CARTESIAN_POINT('Ctrl Pts',(-31.0881307335308,0.296261125619126,
5.46692066132079));
#34607=CARTESIAN_POINT('Ctrl Pts',(-30.9488720894479,-2.36095353548684,
4.93972575908839));
#34608=CARTESIAN_POINT('Ctrl Pts',(-30.809613445365,-4.44014012591879,3.20314655205396));
#34609=CARTESIAN_POINT('Ctrl Pts',(-30.6703548012823,-5.43225507689216,
0.682346650397424));
#34610=CARTESIAN_POINT('Ctrl Pts',(-30.5310961571993,-5.0944006429078,-2.00551097261269));
#34611=CARTESIAN_POINT('Ctrl Pts',(-30.3918375131166,-3.50929312638729,
-4.20236289780168));
#34612=CARTESIAN_POINT('Ctrl Pts',(-30.2525788690337,-1.06501159191773,
-5.37035776096993));
#34613=CARTESIAN_POINT('Ctrl Pts',(-30.1133202249509,1.64001484348643,-5.22353744936069));
#34614=CARTESIAN_POINT('Ctrl Pts',(-29.9740615808681,3.9435193507338,-3.79784771971142));
#34615=CARTESIAN_POINT('Ctrl Pts',(-29.8348029367852,5.2815390029392,-1.44233766232502));
#34616=CARTESIAN_POINT('Ctrl Pts',(-29.6955442927024,5.32648881951606,1.26629736922243));
#34617=CARTESIAN_POINT('Ctrl Pts',(-29.5562856486195,4.0673638165193,3.66490705963996));
#34618=CARTESIAN_POINT('Ctrl Pts',(-29.4170270045367,1.81243333736467,5.1662440485655));
#34619=CARTESIAN_POINT('Ctrl Pts',(-29.2777683604539,-0.886231984291257,
5.40273866124842));
#34620=CARTESIAN_POINT('Ctrl Pts',(-29.138509716371,-3.36792269956474,4.31649034071498));
#34621=CARTESIAN_POINT('Ctrl Pts',(-28.9992510722882,-5.02505086799114,
2.17344333853698));
#34622=CARTESIAN_POINT('Ctrl Pts',(-28.8599924282053,-5.45190473639203,
-0.501723945048768));
#34623=CARTESIAN_POINT('Ctrl Pts',(-28.7207337841225,-4.54397842851747,
-3.05405504418258));
#34624=CARTESIAN_POINT('Ctrl Pts',(-28.5814751400397,-2.52355793355221,
-4.85866725838835));
#34625=CARTESIAN_POINT('Ctrl Pts',(-28.4422164959568,0.114700778743591,
-5.47374057688935));
#34626=CARTESIAN_POINT('Ctrl Pts',(-28.302957851874,2.72487750262012,-4.74868768897724));
#34627=CARTESIAN_POINT('Ctrl Pts',(-28.1636992077911,4.66792729579326,-2.86102200846436));
#34628=CARTESIAN_POINT('Ctrl Pts',(-28.0244405637083,5.46813672032796,-0.272897379119357));
#34629=CARTESIAN_POINT('Ctrl Pts',(-27.8851819196255,4.92959192072193,2.38204023200329));
#34630=CARTESIAN_POINT('Ctrl Pts',(-27.7459232755426,3.18414386600476,4.45378715390773));
#34631=CARTESIAN_POINT('Ctrl Pts',(-27.6066646314598,0.659127510619695,
5.43512125867248));
#34632=CARTESIAN_POINT('Ctrl Pts',(-27.467405987377,-2.02726186526959,5.08578425627286));
#34633=CARTESIAN_POINT('Ctrl Pts',(-27.3281473432941,-4.21732031082938,
3.49130370600942));
#34634=CARTESIAN_POINT('Ctrl Pts',(-27.1888886992113,-5.37485969744026,
1.04205345571222));
#34635=CARTESIAN_POINT('Ctrl Pts',(-27.0496300551285,-5.21648170814461,
-1.66232089571234));
#34636=CARTESIAN_POINT('Ctrl Pts',(-26.9103714110456,-3.78096174542872,
-3.95971216773818));
#34637=CARTESIAN_POINT('Ctrl Pts',(-26.7711127669628,-1.41975561813873,
-5.28765412602722));
#34638=CARTESIAN_POINT('Ctrl Pts',(-26.6318541228799,1.2890467614478,-5.3210290939376));
#34639=CARTESIAN_POINT('Ctrl Pts',(-26.4925954787971,3.68225410651592,-4.05166593721347));
#34640=CARTESIAN_POINT('Ctrl Pts',(-26.3533368347143,5.17394170334293,-1.79034058830659));
#34641=CARTESIAN_POINT('Ctrl Pts',(-26.2140781906314,5.39890232074783,0.909310674496222));
#34642=CARTESIAN_POINT('Ctrl Pts',(-26.0748195465486,4.30205924938349,3.38633701608731));
#34643=CARTESIAN_POINT('Ctrl Pts',(-25.9355609024658,2.15195063489454,5.03429246634581));
#34644=CARTESIAN_POINT('Ctrl Pts',(-25.7963022583829,-0.525016240452773,
5.44971101242903));
#34645=CARTESIAN_POINT('Ctrl Pts',(-25.6570436143001,-3.07344431993646,
4.53088646778747));
#34646=CARTESIAN_POINT('Ctrl Pts',(-25.5177849702172,-4.86940647246544,
2.50277301760284));
#34647=CARTESIAN_POINT('Ctrl Pts',(-25.3785263261344,-5.4732004665362,-0.138089915769586));
#34648=CARTESIAN_POINT('Ctrl Pts',(-25.2392676820516,-4.73700048845459,
-2.74514453974834));
#34649=CARTESIAN_POINT('Ctrl Pts',(-25.1000090379687,-2.84104907436741,
-4.68011029023519));
#34650=CARTESIAN_POINT('Ctrl Pts',(-24.9607503938859,-0.249528649512625,
-5.46925293114166));
#34651=CARTESIAN_POINT('Ctrl Pts',(-24.821491749803,2.4030834324577,-4.91936806799172));
#34652=CARTESIAN_POINT('Ctrl Pts',(-24.6822331057202,4.46735285572938,-3.16508303747874));
#34653=CARTESIAN_POINT('Ctrl Pts',(-24.5429744616374,5.43788819512175,-0.635896335171685));
#34654=CARTESIAN_POINT('Ctrl Pts',(-24.4037158175546,5.07707500320166,2.04897574011852));
#34655=CARTESIAN_POINT('Ctrl Pts',(-24.2644571734717,3.473250534415,4.23220071557519));
#34656=CARTESIAN_POINT('Ctrl Pts',(-24.1251985293889,1.0190762916073,5.37926348895581));
#34657=CARTESIAN_POINT('Ctrl Pts',(-23.985939885306,-1.68459659395356,5.20933071395636));
#34658=CARTESIAN_POINT('Ctrl Pts',(-23.8466812412232,-3.97583268038608,
3.76400673077284));
#34659=CARTESIAN_POINT('Ctrl Pts',(-23.7074225971403,-5.2936726965345,1.39714764921047));
#34660=CARTESIAN_POINT('Ctrl Pts',(-23.5681639530575,-5.31547220635138,
-1.31177261567522));
#34661=CARTESIAN_POINT('Ctrl Pts',(-23.4289053089747,-4.03589407447513,
-3.6995339154204));
#34662=CARTESIAN_POINT('Ctrl Pts',(-23.2896466648919,-1.7682151476239,-5.1815448819288));
#34663=CARTESIAN_POINT('Ctrl Pts',(-23.150388020809,0.932372760685483,-5.39496739627414));
#34664=CARTESIAN_POINT('Ctrl Pts',(-23.0111293767262,3.40468949808556,-4.2875496024367));
#34665=CARTESIAN_POINT('Ctrl Pts',(-22.8718707326433,5.04344213850449,-2.13041863662671));
#34666=CARTESIAN_POINT('Ctrl Pts',(-22.7326120885605,5.44741777672601,0.548298949058622));
#34667=CARTESIAN_POINT('Ctrl Pts',(-22.5933534444776,4.51771177305655,3.09277747458744));
#34668=CARTESIAN_POINT('Ctrl Pts',(-22.4540948003948,2.48194240101049,4.88005677116521));
#34669=CARTESIAN_POINT('Ctrl Pts',(-22.314836156312,-0.161476531273241,
5.47256041552555));
#34670=CARTESIAN_POINT('Ctrl Pts',(-22.1755775122291,-2.76536145052879,
4.72522679028835));
#34671=CARTESIAN_POINT('Ctrl Pts',(-22.0363188681463,-4.69220782584875,
2.82102426270548));
#34672=CARTESIAN_POINT('Ctrl Pts',(-21.8970602240634,-5.47026927337987,
0.226155363511897));
#34673=CARTESIAN_POINT('Ctrl Pts',(-21.7578015799806,-4.90905438758531,
-2.42408275260119));
#34674=CARTESIAN_POINT('Ctrl Pts',(-21.6185429358978,-3.14596441452665,
-4.48083698367404));
#34675=CARTESIAN_POINT('Ctrl Pts',(-21.479284291815,-0.612653548254585,
-5.44055583571572));
#34676=CARTESIAN_POINT('Ctrl Pts',(-21.3400256477321,2.07065220066406,-5.06827304272516));
#34677=CARTESIAN_POINT('Ctrl Pts',(-21.2007670036493,4.24700384032274,-3.45513394125512));
#34678=CARTESIAN_POINT('Ctrl Pts',(-21.0615083595664,5.38356905510338,-0.99608051916624));
#34679=CARTESIAN_POINT('Ctrl Pts',(-20.9222497154836,5.20208459737315,1.70684153145577));
#34680=CARTESIAN_POINT('Ctrl Pts',(-20.7829910714008,3.74698298534229,3.99188059431702));
#34681=CARTESIAN_POINT('Ctrl Pts',(-20.6437324273179,1.3745141683616,5.29959460456198));
#34682=CARTESIAN_POINT('Ctrl Pts',(-20.5044737832351,-1.33447451693076,
5.30981825822612));
#34683=CARTESIAN_POINT('Ctrl Pts',(-20.3652151391523,-3.71674617082413,
4.02004851629844));
#34684=CARTESIAN_POINT('Ctrl Pts',(-20.2259564950694,-5.18905344548906,
1.74605741932713));
#34685=CARTESIAN_POINT('Ctrl Pts',(-20.0866978509866,-5.39093395967906,
-0.955417821745186));
#34686=CARTESIAN_POINT('Ctrl Pts',(-19.9474392069037,-4.27296166482091,
-3.42297981044299));
#34687=CARTESIAN_POINT('Ctrl Pts',(-19.8081805628209,-2.10884773690798,
-5.05249971739409));
#34688=CARTESIAN_POINT('Ctrl Pts',(-19.6689219187381,0.57157164572401,-5.44502507115747));
#34689=CARTESIAN_POINT('Ctrl Pts',(-19.5296632746552,3.11205415511225,-4.50445458489459));
#34690=CARTESIAN_POINT('Ctrl Pts',(-19.3904046305724,4.89061796001327,-2.4610664641421));
#34691=CARTESIAN_POINT('Ctrl Pts',(-19.2511459864896,5.47182043554474,0.184860198215039));
#34692=CARTESIAN_POINT('Ctrl Pts',(-19.1118873424067,4.71336680946623,2.78552786580056));
#34693=CARTESIAN_POINT('Ctrl Pts',(-18.9726286983239,2.80094793913186,4.7042196817328));
#34694=CARTESIAN_POINT('Ctrl Pts',(-18.833370054241,0.202777947913637,5.47118572848419));
#34695=CARTESIAN_POINT('Ctrl Pts',(-18.6941114101582,-2.44503780898611,
4.89865106783058));
#34696=CARTESIAN_POINT('Ctrl Pts',(-18.5548527660754,-4.4942392915216,3.12678834625449));
#34697=CARTESIAN_POINT('Ctrl Pts',(-18.4155941219925,-5.44312413174327,
0.589399574281588));
#34698=CARTESIAN_POINT('Ctrl Pts',(-18.2763354779097,-5.05937853556709,
-2.09229085109412));
#34699=CARTESIAN_POINT('Ctrl Pts',(-18.1370768338268,-3.43695425733871,
-4.26172941476702));
#34700=CARTESIAN_POINT('Ctrl Pts',(-17.997818189744,-0.973066558291814,
-5.3877763172633));
#34701=CARTESIAN_POINT('Ctrl Pts',(-17.8585595456612,1.72905530202626,-5.19474349070905));
#34702=CARTESIAN_POINT('Ctrl Pts',(-17.7193009015783,4.00785561649581,-3.7298908199909));
#34703=CARTESIAN_POINT('Ctrl Pts',(-17.5800422574955,5.30541974197549,-1.35185558887996));
#34704=CARTESIAN_POINT('Ctrl Pts',(-17.4407836134126,5.30406735280308,1.35715205067734));
#34705=CARTESIAN_POINT('Ctrl Pts',(-17.3015249693298,4.00412955202339,3.73389055843128));
#34706=CARTESIAN_POINT('Ctrl Pts',(-17.162266325247,1.72386780801632,5.19646725691738));
#34707=CARTESIAN_POINT('Ctrl Pts',(-17.0230076811642,-0.978445436872712,
5.38680208461312));
#34708=CARTESIAN_POINT('Ctrl Pts',(-16.8837490370813,-3.44120761917852,
4.25829570291177));
#34709=CARTESIAN_POINT('Ctrl Pts',(-16.7444903929985,-5.06146503762314,
2.08723832962307));
#34710=CARTESIAN_POINT('Ctrl Pts',(-16.6052317489156,-5.44253293941428,
-0.59483390548928));
#34711=CARTESIAN_POINT('Ctrl Pts',(-16.4659731048328,-4.491115145378,-3.13127400951843));
#34712=CARTESIAN_POINT('Ctrl Pts',(-16.3267144607499,-2.4401455881925,-4.90108984616219));
#34713=CARTESIAN_POINT('Ctrl Pts',(-16.1874558166671,0.208240489609049,
-5.47098054010582));
#34714=CARTESIAN_POINT('Ctrl Pts',(-16.0481971725843,2.8056434173249,-4.70142076255153));
#34715=CARTESIAN_POINT('Ctrl Pts',(-15.9089385285015,4.71614563855093,-2.78082047024009));
#34716=CARTESIAN_POINT('Ctrl Pts',(-15.7696798844186,5.47200227972015,-0.179396829589313));
#34717=CARTESIAN_POINT('Ctrl Pts',(-15.6304212403358,4.88815829869211,2.4659482189731));
#34718=CARTESIAN_POINT('Ctrl Pts',(-15.4911625962529,3.10755518281749,4.50755953454565));
#34719=CARTESIAN_POINT('Ctrl Pts',(-15.3519039521701,0.566134837870747,
5.44559303630728));
#34720=CARTESIAN_POINT('Ctrl Pts',(-15.2126453080873,-2.11389129628661,
5.05039164414136));
#34721=CARTESIAN_POINT('Ctrl Pts',(-15.0733866640044,-4.27637717001899,
3.41871181462692));
#34722=CARTESIAN_POINT('Ctrl Pts',(-14.9341280199216,-5.39188519861101,
0.950034829218862));
#34723=CARTESIAN_POINT('Ctrl Pts',(-14.7948693758387,-5.18730752801265,
-1.75123750004177));
#34724=CARTESIAN_POINT('Ctrl Pts',(-14.6556107317559,-3.71273054682144,
-4.02375745521871));
#34725=CARTESIAN_POINT('Ctrl Pts',(-14.5163520876731,-1.32917232451103,
-5.31114800240805));
#34726=CARTESIAN_POINT('Ctrl Pts',(-14.3770934435902,1.37980480282327,-5.29821959509371));
#34727=CARTESIAN_POINT('Ctrl Pts',(-14.2378347995074,3.7509667651852,-3.98813747233033));
#34728=CARTESIAN_POINT('Ctrl Pts',(-14.0985761554246,5.2037861808374,-1.70164671887413));
#34729=CARTESIAN_POINT('Ctrl Pts',(-13.9593175113417,5.38257184652445,1.00145518558331));
#34730=CARTESIAN_POINT('Ctrl Pts',(-13.8200588672589,4.24355198451,3.45937259145215));
#34731=CARTESIAN_POINT('Ctrl Pts',(-13.680800223176,2.0655908093598,5.07033793548493));
#34732=CARTESIAN_POINT('Ctrl Pts',(-13.5415415790932,-0.618085303585742,
5.43994142700276));
#34733=CARTESIAN_POINT('Ctrl Pts',(-13.4022829350104,-3.15043668685167,
4.47769369808479));
#34734=CARTESIAN_POINT('Ctrl Pts',(-13.2630242909275,-4.91147223839532,
2.41918015517678));
#34735=CARTESIAN_POINT('Ctrl Pts',(-13.1237656468447,-5.47004074454526,
-0.231616978531012));
#34736=CARTESIAN_POINT('Ctrl Pts',(-12.9845070027618,-4.68938886767918,
-2.82570773779167));
#34737=CARTESIAN_POINT('Ctrl Pts',(-12.845248358679,-2.760642223558,-4.72798547853501));
#34738=CARTESIAN_POINT('Ctrl Pts',(-12.7059897145962,-0.15601243547838,
-5.47271891217753));
#34739=CARTESIAN_POINT('Ctrl Pts',(-12.5667310705134,2.48681360073797,-4.87757627176797));
#34740=CARTESIAN_POINT('Ctrl Pts',(-12.4274724264305,4.52079746951866,-3.08826527541316));
#34741=CARTESIAN_POINT('Ctrl Pts',(-12.2882137823477,5.44796250432556,-0.54285976383591));
#34742=CARTESIAN_POINT('Ctrl Pts',(-12.1489551382648,5.04131253254851,2.13545314181759));
#34743=CARTESIAN_POINT('Ctrl Pts',(-12.009696494182,3.40040694622673,4.29094683861058));
#34744=CARTESIAN_POINT('Ctrl Pts',(-11.8704378500992,0.926985752507082,
5.39589562411822));
#34745=CARTESIAN_POINT('Ctrl Pts',(-11.7311792060163,-1.77338772045491,
5.17977684506475));
#34746=CARTESIAN_POINT('Ctrl Pts',(-11.5919205619335,-4.0395858201179,3.69550247918081));
#34747=CARTESIAN_POINT('Ctrl Pts',(-11.4526619178506,-5.31677928126165,
1.30646478945133));
#34748=CARTESIAN_POINT('Ctrl Pts',(-11.3134032737678,-5.2922750918781,-1.40243235972937));
#34749=CARTESIAN_POINT('Ctrl Pts',(-11.174144629685,-3.9720725692345,-3.76797447927451));
#34750=CARTESIAN_POINT('Ctrl Pts',(-11.0348859856021,-1.67939455765743,
-5.21101008360564));
#34751=CARTESIAN_POINT('Ctrl Pts',(-10.8956273415193,1.02444664771917,-5.37824332265714));
#34752=CARTESIAN_POINT('Ctrl Pts',(-10.7563686974365,3.47747439557152,-4.22873077883584));
#34753=CARTESIAN_POINT('Ctrl Pts',(-10.6171100533536,5.07911824896027,-2.04390557140199));
#34754=CARTESIAN_POINT('Ctrl Pts',(-10.4778514092708,5.43725058124388,0.641325415442486));
#34755=CARTESIAN_POINT('Ctrl Pts',(-10.3385927651879,4.46419048809091,3.16954183720107));
#34756=CARTESIAN_POINT('Ctrl Pts',(-10.1993341211051,2.39817054792408,4.92176494713011));
#34757=CARTESIAN_POINT('Ctrl Pts',(-10.0600754770223,-0.254989238126229,
5.46900106602376));
#34758=CARTESIAN_POINT('Ctrl Pts',(-9.92081683293943,-2.84572046082652,
4.67727134455151));
#34759=CARTESIAN_POINT('Ctrl Pts',(-9.78155818885659,-4.73973898548971,
2.74041356754016));
#34760=CARTESIAN_POINT('Ctrl Pts',(-9.64229954477374,-5.47333561277054,
0.132625192579784));
#34761=CARTESIAN_POINT('Ctrl Pts',(-9.50304090069093,-4.86690518028598,
-2.50763357327872));
#34762=CARTESIAN_POINT('Ctrl Pts',(-9.36378225660807,-3.06891897627543,
-4.53395285471581));
#34763=CARTESIAN_POINT('Ctrl Pts',(-9.22452361252525,-0.519574777180205,
-5.45023249253162));
#34764=CARTESIAN_POINT('Ctrl Pts',(-9.0852649684424,2.15697599396752,-5.0321413665732));
#34765=CARTESIAN_POINT('Ctrl Pts',(-8.94600632435957,4.30543815449961,-3.38203998638518));
#34766=CARTESIAN_POINT('Ctrl Pts',(-8.80674768027672,5.39980752055461,-0.903919749032533));
#34767=CARTESIAN_POINT('Ctrl Pts',(-8.66748903619389,5.17215157937558,1.79550555880287));
#34768=CARTESIAN_POINT('Ctrl Pts',(-8.52823039211106,3.67820693165339,4.05534042216757));
#34769=CARTESIAN_POINT('Ctrl Pts',(-8.38897174802822,1.28373339834046,5.32231347570908));
#34770=CARTESIAN_POINT('Ctrl Pts',(-8.24971310394538,-1.42503430821612,
5.28623395170288));
#34771=CARTESIAN_POINT('Ctrl Pts',(-8.11045445986255,-3.784913390138,3.9559351360814));
#34772=CARTESIAN_POINT('Ctrl Pts',(-7.9711958157797,-5.21813883331359,1.65711173069105));
#34773=CARTESIAN_POINT('Ctrl Pts',(-7.83193717169687,-5.3738165920501,-1.04741940345607));
#34774=CARTESIAN_POINT('Ctrl Pts',(-7.69267852761403,-4.21383235652447,
-3.49551270099778));
#34775=CARTESIAN_POINT('Ctrl Pts',(-7.55341988353118,-2.02218301172191,
-5.0878058177207));
#34776=CARTESIAN_POINT('Ctrl Pts',(-7.41416123944835,0.664553816695306,
-5.43446045127249));
#34777=CARTESIAN_POINT('Ctrl Pts',(-7.27490259536552,3.18858911170672,-4.45060576196482));
#34778=CARTESIAN_POINT('Ctrl Pts',(-7.13564395128268,4.93196778442169,-2.37711715006973));
#34779=CARTESIAN_POINT('Ctrl Pts',(-6.99638530719984,5.46786152352583,0.278356841617121));
#34780=CARTESIAN_POINT('Ctrl Pts',(-6.85712666311701,4.66506841443464,2.86568122099679));
#34781=CARTESIAN_POINT('Ctrl Pts',(-6.71786801903417,2.72013487156228,4.75140594479573));
#34782=CARTESIAN_POINT('Ctrl Pts',(-6.57860937495132,0.109235527944913,
5.47385237023832));
#34783=CARTESIAN_POINT('Ctrl Pts',(-6.43935073086849,-2.52840775642265,
4.85614521910033));
#34784=CARTESIAN_POINT('Ctrl Pts',(-6.30009208678566,-4.54702544991989,
3.04951663866756));
#34785=CARTESIAN_POINT('Ctrl Pts',(-6.1608334427028,-5.45240295947547,0.496280303087244));
#34786=CARTESIAN_POINT('Ctrl Pts',(-6.02157479861998,-5.02287831368086,
-2.17845945972919));
#34787=CARTESIAN_POINT('Ctrl Pts',(-5.88231615453714,-3.36361127048301,
-4.31985085307454));
#34788=CARTESIAN_POINT('Ctrl Pts',(-5.74305751045431,-0.880837239980666,
-5.40362081648892));
#34789=CARTESIAN_POINT('Ctrl Pts',(-5.60379886637147,1.81759061121365,-5.16443187018255));
#34790=CARTESIAN_POINT('Ctrl Pts',(-5.46454022228863,4.07102097368853,-3.66084422005602));
#34791=CARTESIAN_POINT('Ctrl Pts',(-5.32528157820578,5.32775048469594,-1.26097856625377));
#34792=CARTESIAN_POINT('Ctrl Pts',(-5.18602293412295,5.2800962848793,1.44761023557204));
#34793=CARTESIAN_POINT('Ctrl Pts',(-5.04676429004012,3.93972546754036,3.80178318847132));
#34794=CARTESIAN_POINT('Ctrl Pts',(-4.90750564595728,1.63479864485923,5.22517229979028));
#34795=CARTESIAN_POINT('Ctrl Pts',(-4.76824700187443,-1.07037303331147,
5.36929173553541));
#34796=CARTESIAN_POINT('Ctrl Pts',(-4.62898835779161,-3.51348717835118,
4.19885698962121));
#34797=CARTESIAN_POINT('Ctrl Pts',(-4.48972971370876,-5.09640048313106,
2.000423526974));
#34798=CARTESIAN_POINT('Ctrl Pts',(-4.35047106962593,-5.43157108803641,
-0.6877700831933));
#34799=CARTESIAN_POINT('Ctrl Pts',(-4.21121242554309,-4.43693976776381,
-3.20757816256517));
#34800=CARTESIAN_POINT('Ctrl Pts',(-4.07195378146025,-2.35602034604859,
-4.94208056396663));
#34801=CARTESIAN_POINT('Ctrl Pts',(-3.93269513737741,0.30171936231118,-5.46662213785894));
#34802=CARTESIAN_POINT('Ctrl Pts',(-3.79343649329457,2.88558965381968,-4.65278030015506));
#34803=CARTESIAN_POINT('Ctrl Pts',(-3.65417784921175,4.76298614341351,-2.69980650591098));
#34804=CARTESIAN_POINT('Ctrl Pts',(-3.5149192051289,5.47426917514671,-0.0858438686731754));
#34805=CARTESIAN_POINT('Ctrl Pts',(-3.37566056104607,4.8452965846843,2.54913577084127));
#34806=CARTESIAN_POINT('Ctrl Pts',(-3.23640191696323,3.03005861688361,4.56001501640902));
#34807=CARTESIAN_POINT('Ctrl Pts',(-3.09714327288038,0.47297676690079,5.45447386555561));
#34808=CARTESIAN_POINT('Ctrl Pts',(-2.95788462879755,-2.19990314678726,
5.01352354295405));
#34809=CARTESIAN_POINT('Ctrl Pts',(-2.81862598471472,-4.33418467121216,
3.34512113514759));
#34810=CARTESIAN_POINT('Ctrl Pts',(-2.67936734063187,-5.40733544218769,
0.857738646605811));
#34811=CARTESIAN_POINT('Ctrl Pts',(-2.54010869654903,-5.15661785864793,
-1.83964247396158));
#34812=CARTESIAN_POINT('Ctrl Pts',(-2.4008500524662,-3.64341466104068,-4.08662718923746));
#34813=CARTESIAN_POINT('Ctrl Pts',(-2.26159140838337,-1.23820070945758,
-5.33309020721854));
#34814=CARTESIAN_POINT('Ctrl Pts',(-2.12233276430052,1.4701597310491,-5.2738622068446));
#34815=CARTESIAN_POINT('Ctrl Pts',(-1.98307412021769,3.81858356332732,-3.92344385303797));
#34816=CARTESIAN_POINT('Ctrl Pts',(-1.84381547613485,5.2321103602713,-1.6124557204024));
#34817=CARTESIAN_POINT('Ctrl Pts',(-1.704556832052,5.36466882468081,1.09330714313199));
#34818=CARTESIAN_POINT('Ctrl Pts',(-1.56529818796917,4.18380497314764,3.53139745068011));
#34819=CARTESIAN_POINT('Ctrl Pts',(-1.42603954388634,1.97862747239897,5.10490218334346));
#34820=CARTESIAN_POINT('Ctrl Pts',(-1.28678089980349,-0.710973708892522,
5.42858235876716));
#34821=CARTESIAN_POINT('Ctrl Pts',(-1.14752225572066,-3.22650880324846,
4.42319311700711));
#34822=CARTESIAN_POINT('Ctrl Pts',(-1.00826361163783,-4.95210278852054,
2.33487981484443));
#34823=CARTESIAN_POINT('Ctrl Pts',(-0.869004967554984,-5.46528354152855,
-0.325074995677754));
#34824=CARTESIAN_POINT('Ctrl Pts',(-0.729746323472146,-4.64040603618749,
-2.90544808420485));
#34825=CARTESIAN_POINT('Ctrl Pts',(-0.59048767938932,-2.67943116337464,
-4.77447412454503));
#34826=CARTESIAN_POINT('Ctrl Pts',(-0.451229035306469,-0.0624461122722286,
-5.47459625409955));
#34827=CARTESIAN_POINT('Ctrl Pts',(-0.31197039122363,2.56980840002131,-4.83433950546158));
#34828=CARTESIAN_POINT('Ctrl Pts',(-0.172711747140798,4.57293856493704,
-3.01058424967472));
#34829=CARTESIAN_POINT('Ctrl Pts',(-0.0334531030579653,5.45641147518307,
-0.449588311427022));
#34830=CARTESIAN_POINT('Ctrl Pts',(0.105805541024878,5.0041434537287,2.22115548407858));
#34831=CARTESIAN_POINT('Ctrl Pts',(0.245064185107707,3.3264356378341,4.34875895322203));
#34832=CARTESIAN_POINT('Ctrl Pts',(0.337903281162932,1.66543784564298,5.05629436626422));
#34833=CARTESIAN_POINT('Ctrl Pts',(0.384322829190546,0.800498355117692,
5.18970890870239));
#34834=CARTESIAN_POINT('Ctrl Pts',(-59.58325,2.85706463458446,-4.00329423553987));
#34835=CARTESIAN_POINT('Ctrl Pts',(-59.5368304519724,3.52427108824591,-3.52712339958193));
#34836=CARTESIAN_POINT('Ctrl Pts',(-59.4439913559172,4.61530848209962,-2.23520568907806));
#34837=CARTESIAN_POINT('Ctrl Pts',(-59.3047327118343,5.12174738739822,0.251511598513074));
#34838=CARTESIAN_POINT('Ctrl Pts',(-59.1654740677515,4.3742789497841,2.67597888304926));
#34839=CARTESIAN_POINT('Ctrl Pts',(-59.0262154236687,2.55584624568566,4.44562215581043));
#34840=CARTESIAN_POINT('Ctrl Pts',(-58.8869567795858,0.111678748687467,
5.12668320818063));
#34841=CARTESIAN_POINT('Ctrl Pts',(-58.747698135503,-2.35983518894881,4.55267369514457));
#34842=CARTESIAN_POINT('Ctrl Pts',(-58.60843949142,-4.25359264236838,2.86399697899764));
#34843=CARTESIAN_POINT('Ctrl Pts',(-58.4691808473374,-5.10595168183977,
0.474155594652121));
#34844=CARTESIAN_POINT('Ctrl Pts',(-58.3299222032543,-4.70822903633895,
-2.03178406622669));
#34845=CARTESIAN_POINT('Ctrl Pts',(-58.1906635591718,-3.15779931679017,
-4.04027968761638));
#34846=CARTESIAN_POINT('Ctrl Pts',(-58.0514049150887,-0.834251032978302,
-5.05960384006236));
#34847=CARTESIAN_POINT('Ctrl Pts',(-57.9121462710061,1.69354537464531,-4.84019258737259));
#34848=CARTESIAN_POINT('Ctrl Pts',(-57.772887626923,3.8067141091864,-3.43576636062821));
#34849=CARTESIAN_POINT('Ctrl Pts',(-57.6336289828404,4.98789175297897,-1.19016713333119));
#34850=CARTESIAN_POINT('Ctrl Pts',(-57.4943703387573,4.94789270758304,1.34681839400263));
#34851=CARTESIAN_POINT('Ctrl Pts',(-57.3551116946747,3.69650985244822,3.55406486819218));
#34852=CARTESIAN_POINT('Ctrl Pts',(-57.2158530505917,1.54011704282762,4.89117588296368));
#34853=CARTESIAN_POINT('Ctrl Pts',(-57.076594406509,-0.993339894845993,
5.03078900139859));
#34854=CARTESIAN_POINT('Ctrl Pts',(-56.937335762426,-3.28359918545446,3.93872294825806));
#34855=CARTESIAN_POINT('Ctrl Pts',(-56.7980771183433,-4.76994070613421,
1.88234634223453));
#34856=CARTESIAN_POINT('Ctrl Pts',(-56.6588184742604,-5.08846609548997,
-0.634881787205557));
#34857=CARTESIAN_POINT('Ctrl Pts',(-56.5195598301776,-4.1611913471364,-2.99667293168903));
#34858=CARTESIAN_POINT('Ctrl Pts',(-56.3803011860948,-2.21513949450856,
-4.62479395317148));
#34859=CARTESIAN_POINT('Ctrl Pts',(-56.2410425420119,0.273241035485556,
-5.12063486534734));
#34860=CARTESIAN_POINT('Ctrl Pts',(-56.1017838979291,2.69472444693603,-4.36279981705527));
#34861=CARTESIAN_POINT('Ctrl Pts',(-55.9625252538462,4.45646324687071,-2.53682821994801));
#34862=CARTESIAN_POINT('Ctrl Pts',(-55.8232666097634,5.1271340465709,-0.089769464874975));
#34863=CARTESIAN_POINT('Ctrl Pts',(-55.6840079656806,4.54253770251526,2.37926738925458));
#34864=CARTESIAN_POINT('Ctrl Pts',(-55.5447493215977,2.84579990176412,4.26579242432466));
#34865=CARTESIAN_POINT('Ctrl Pts',(-55.4054906775149,0.452329953591429,
5.1079310587967));
#34866=CARTESIAN_POINT('Ctrl Pts',(-55.266232033432,-2.05188313562661,4.69950398298055));
#34867=CARTESIAN_POINT('Ctrl Pts',(-55.1269733893492,-4.0537373125207,3.14050567415567));
#34868=CARTESIAN_POINT('Ctrl Pts',(-54.9877147452663,-5.06312216608579,
0.812622925848719));
#34869=CARTESIAN_POINT('Ctrl Pts',(-54.8484561011836,-4.83291179117217,
-1.71421285349086));
#34870=CARTESIAN_POINT('Ctrl Pts',(-54.7091974571006,-3.41946818595568,
-3.82136093735749));
#34871=CARTESIAN_POINT('Ctrl Pts',(-54.5699388130178,-1.16884224379346,
-4.99293199407404));
#34872=CARTESIAN_POINT('Ctrl Pts',(-54.430680168935,1.36794927382256,-4.94209235775424));
#34873=CARTESIAN_POINT('Ctrl Pts',(-54.2914215248522,3.56982819462436,-3.68128900647443));
#34874=CARTESIAN_POINT('Ctrl Pts',(-54.1521628807693,4.89771240398387,-1.51920219068664));
#34875=CARTESIAN_POINT('Ctrl Pts',(-54.0129042366865,5.02649836382728,1.01482820554322));
#34876=CARTESIAN_POINT('Ctrl Pts',(-53.8736455926037,3.9246556358045,3.30040001040366));
#34877=CARTESIAN_POINT('Ctrl Pts',(-53.7343869485209,1.86194642264088,4.77794072875955));
#34878=CARTESIAN_POINT('Ctrl Pts',(-53.5951283044379,-0.656619833959052,
5.08570668461877));
#34879=CARTESIAN_POINT('Ctrl Pts',(-53.4558696603552,-3.01442702008815,
4.14834808434477));
#34880=CARTESIAN_POINT('Ctrl Pts',(-53.3166110162723,-4.63421738021059,
2.19535677311881));
#34881=CARTESIAN_POINT('Ctrl Pts',(-53.1773523721895,-5.11942051059543,
-0.295119846874734));
#34882=CARTESIAN_POINT('Ctrl Pts',(-53.0380937281066,-4.35124498857135,
-2.71334279768651));
#34883=CARTESIAN_POINT('Ctrl Pts',(-52.8988350840238,-2.51776186605044,
-4.46726283916524));
#34884=CARTESIAN_POINT('Ctrl Pts',(-52.759576439941,-0.0678595671353494,
-5.12747083536052));
#34885=CARTESIAN_POINT('Ctrl Pts',(-52.6203177958581,2.39865666935982,-4.53232923239918));
#34886=CARTESIAN_POINT('Ctrl Pts',(-52.4810591517753,4.27791404372175,-2.82754549439134));
#34887=CARTESIAN_POINT('Ctrl Pts',(-52.3418005076925,5.10981730287787,-0.430498803174167));
#34888=CARTESIAN_POINT('Ctrl Pts',(-52.2025418636096,4.69069304595447,2.07194614721496));
#34889=CARTESIAN_POINT('Ctrl Pts',(-52.0632832195268,3.12315472211971,4.06712019370289));
#34890=CARTESIAN_POINT('Ctrl Pts',(-51.924024575444,0.790979961646617,5.06654840977544));
#34891=CARTESIAN_POINT('Ctrl Pts',(-51.7847659313611,-1.73484902128376,
4.82554255619773));
#34892=CARTESIAN_POINT('Ctrl Pts',(-51.6455072872782,-3.83593799234573,
3.40310766905826));
#34893=CARTESIAN_POINT('Ctrl Pts',(-51.5062486431955,-4.99788106171436,
1.14749596133553));
#34894=CARTESIAN_POINT('Ctrl Pts',(-51.3669899991126,-4.93620176658556,
-1.3890551493307));
#34895=CARTESIAN_POINT('Ctrl Pts',(-51.2277313550298,-3.66600093949493,
-3.58552634907998));
#34896=CARTESIAN_POINT('Ctrl Pts',(-51.0884727109469,-1.49825959824569,
-4.90415948604745));
#34897=CARTESIAN_POINT('Ctrl Pts',(-50.9492140668641,1.03629798564688,-5.02211594582091));
#34898=CARTESIAN_POINT('Ctrl Pts',(-50.8099554227812,3.31714056994997,-3.91051665736339));
#34899=CARTESIAN_POINT('Ctrl Pts',(-50.6706967786984,4.78585350621771,-1.84151250480363));
#34900=CARTESIAN_POINT('Ctrl Pts',(-50.5314381346155,5.08285440870451,0.678345891295609));
#34901=CARTESIAN_POINT('Ctrl Pts',(-50.3921794905327,4.13542907271616,3.03212606480312));
#34902=CARTESIAN_POINT('Ctrl Pts',(-50.2529208464499,2.17553396450143,4.64355618654767));
#34903=CARTESIAN_POINT('Ctrl Pts',(-50.113662202367,-0.316993269371489,
5.11811267514673));
#34904=CARTESIAN_POINT('Ctrl Pts',(-49.9744035582842,-2.73191160279071,
4.33961070637241));
#34905=CARTESIAN_POINT('Ctrl Pts',(-49.8351449142014,-4.47798085922564,
2.49864953779702));
#34906=CARTESIAN_POINT('Ctrl Pts',(-49.6958862701186,-5.12771399651721,
0.0459484302882166));
#34907=CARTESIAN_POINT('Ctrl Pts',(-49.5566276260356,-4.52203800193704,
-2.41800214999114));
#34908=CARTESIAN_POINT('Ctrl Pts',(-49.4173689819529,-2.80923945602917,
-4.28995754839293));
#34909=CARTESIAN_POINT('Ctrl Pts',(-49.27811033787,-0.408659791847362,-5.11161024168038));
#34910=CARTESIAN_POINT('Ctrl Pts',(-49.1388516937872,2.09197132506023,-4.68179645685823));
#34911=CARTESIAN_POINT('Ctrl Pts',(-48.9995930497043,4.08042880925776,-3.10574674126912));
#34912=CARTESIAN_POINT('Ctrl Pts',(-48.8603344056215,5.06988213827541,-0.769322554147787));
#34913=CARTESIAN_POINT('Ctrl Pts',(-48.7210757615387,4.81808520680125,1.75545351072806));
#34914=CARTESIAN_POINT('Ctrl Pts',(-48.5818171174558,3.38668501140426,3.85044500309434));
#34915=CARTESIAN_POINT('Ctrl Pts',(-48.442558473373,1.12612872559781,5.00273886803099));
#34916=CARTESIAN_POINT('Ctrl Pts',(-48.3032998292901,-1.4101356606875,4.93022104035731));
#34917=CARTESIAN_POINT('Ctrl Pts',(-48.1640411852073,-3.60115903181333,
3.65064593132692));
#34918=CARTESIAN_POINT('Ctrl Pts',(-48.0247825411245,-4.91051701814359,
1.47728964757986));
#34919=CARTESIAN_POINT('Ctrl Pts',(-47.8855238970416,-5.0176418239618,-1.05774884294608));
#34920=CARTESIAN_POINT('Ctrl Pts',(-47.7462652529588,-3.89630627287599,
-3.33382055849918));
#34921=CARTESIAN_POINT('Ctrl Pts',(-47.607006608876,-1.82104496094234,-4.79367889397601));
#34922=CARTESIAN_POINT('Ctrl Pts',(-47.4677479647931,0.700059562034036,
-5.07990931985298));
#34923=CARTESIAN_POINT('Ctrl Pts',(-47.3284893207103,3.04976974288669,-4.12243454813989));
#34924=CARTESIAN_POINT('Ctrl Pts',(-47.1892306766275,4.65281020153438,-2.15567143062717));
#34925=CARTESIAN_POINT('Ctrl Pts',(-47.0499720325446,5.11671138294472,0.33886090357014));
#34926=CARTESIAN_POINT('Ctrl Pts',(-46.9107133884618,4.32789718286852,2.75043052318056));
#34927=CARTESIAN_POINT('Ctrl Pts',(-46.771454744379,2.47949158419529,4.48861711134167));
#34928=CARTESIAN_POINT('Ctrl Pts',(-46.6321961002961,0.0240364544226033,
5.12786352560043));
#34929=CARTESIAN_POINT('Ctrl Pts',(-46.4929374562133,-2.43730347789571,
4.51166419904695));
#34930=CARTESIAN_POINT('Ctrl Pts',(-46.3536788121304,-4.30192271842598,
2.79088212094582));
#34931=CARTESIAN_POINT('Ctrl Pts',(-46.2144201680476,-5.11330984246402,
0.386813318391489));
#34932=CARTESIAN_POINT('Ctrl Pts',(-46.0751615239648,-4.67281437814416,
-2.11195830350261));
#34933=CARTESIAN_POINT('Ctrl Pts',(-45.9359028798819,-3.0882820494734,-4.09366291616992));
#34934=CARTESIAN_POINT('Ctrl Pts',(-45.7966442357991,-0.747651098816729,
-5.07312329071181));
#34935=CARTESIAN_POINT('Ctrl Pts',(-45.6573855917162,1.77602594558582,-4.81053987915395));
#34936=CARTESIAN_POINT('Ctrl Pts',(-45.5181269476334,3.86488170470528,-3.37020051287143));
#34937=CARTESIAN_POINT('Ctrl Pts',(-45.3788683035506,5.00750532432036,-1.10474092674605));
#34938=CARTESIAN_POINT('Ctrl Pts',(-45.2396096594678,4.92415028827758,1.43119042296277));
#34939=CARTESIAN_POINT('Ctrl Pts',(-45.1003510153849,3.63522426235287,3.61672595737161));
#34940=CARTESIAN_POINT('Ctrl Pts',(-44.9610923713021,1.45629272160045,4.91678488418377));
#34941=CARTESIAN_POINT('Ctrl Pts',(-44.8218337272192,-1.07918038574816,
5.01307607994741));
#34942=CARTESIAN_POINT('Ctrl Pts',(-44.6825750831364,-3.35043967147466,
3.88202474182395));
#34943=CARTESIAN_POINT('Ctrl Pts',(-44.5433164390536,-4.80141674914282,
1.80054416479442));
#34944=CARTESIAN_POINT('Ctrl Pts',(-44.4040577949707,-5.07687147184152,
-0.721760449682717));
#34945=CARTESIAN_POINT('Ctrl Pts',(-44.2647991508879,-4.10936474789597,
-3.06735773216533));
#34946=CARTESIAN_POINT('Ctrl Pts',(-44.125540506805,-2.13576953418586,-4.66197925619238));
#34947=CARTESIAN_POINT('Ctrl Pts',(-43.9862818627222,0.360722350167653,
-5.11521665957699));
#34948=CARTESIAN_POINT('Ctrl Pts',(-43.8470232186393,2.7688992207005,-4.31610463194866));
#34949=CARTESIAN_POINT('Ctrl Pts',(-43.7077645745566,4.49917140129531,-2.46028835506957));
#34950=CARTESIAN_POINT('Ctrl Pts',(-43.5685059304736,5.12791941987977,-0.00212403965129634));
#34951=CARTESIAN_POINT('Ctrl Pts',(-43.4292472863909,4.50120801315461,2.4565603006312));
#34952=CARTESIAN_POINT('Ctrl Pts',(-43.289988642308,2.77247382434629,4.31380933533684));
#34953=CARTESIAN_POINT('Ctrl Pts',(-43.1507299982252,0.364959781723236,
5.11491607419408));
#34954=CARTESIAN_POINT('Ctrl Pts',(-43.0114713541423,-2.13190671757982,
4.66374697382507));
#34955=CARTESIAN_POINT('Ctrl Pts',(-42.8722127100594,-4.10682227278453,
3.0707609656379));
#34956=CARTESIAN_POINT('Ctrl Pts',(-42.7329540659767,-5.0762718079012,0.72596599137429));
#34957=CARTESIAN_POINT('Ctrl Pts',(-42.5936954218938,-4.80290671103353,
-1.79656595020431));
#34958=CARTESIAN_POINT('Ctrl Pts',(-42.454436777811,-3.35365447446679,-3.87924783356431));
#34959=CARTESIAN_POINT('Ctrl Pts',(-42.3151781337281,-1.08333295532153,
-5.01218034354698));
#34960=CARTESIAN_POINT('Ctrl Pts',(-42.1759194896453,1.45221905169649,-4.91798962119831));
#34961=CARTESIAN_POINT('Ctrl Pts',(-42.0366608455625,3.63222684150266,-3.61973621417252));
#34962=CARTESIAN_POINT('Ctrl Pts',(-41.8974022014796,4.9229629697167,-1.43526920371147));
#34963=CARTESIAN_POINT('Ctrl Pts',(-41.7581435573968,5.00841879714827,1.10059222271303));
#34964=CARTESIAN_POINT('Ctrl Pts',(-41.618884913314,3.8676723249881,3.36699760541134));
#34965=CARTESIAN_POINT('Ctrl Pts',(-41.4796262692311,1.78001049070443,4.80906693042493));
#34966=CARTESIAN_POINT('Ctrl Pts',(-41.3403676251483,-0.743448157983408,
5.07374092014123));
#34967=CARTESIAN_POINT('Ctrl Pts',(-41.2011089810654,-3.08488971148233,
4.09621991063895));
#34968=CARTESIAN_POINT('Ctrl Pts',(-41.0618503369826,-4.67106318309472,
2.11582863858619));
#34969=CARTESIAN_POINT('Ctrl Pts',(-40.9225916928997,-5.11362853233719,
-0.382577209973956));
#34970=CARTESIAN_POINT('Ctrl Pts',(-40.7833330488169,-4.30423326894481,
-2.78731735811214));
#34971=CARTESIAN_POINT('Ctrl Pts',(-40.6440744047341,-2.4410402010708,-4.50964353636523));
#34972=CARTESIAN_POINT('Ctrl Pts',(-40.5048157606512,0.0197884139050482,
-5.12788167833459));
#34973=CARTESIAN_POINT('Ctrl Pts',(-40.3655571165684,2.47577226656799,-4.49066963518998));
#34974=CARTESIAN_POINT('Ctrl Pts',(-40.2262984724856,4.32561718207586,-2.75401490236612));
#34975=CARTESIAN_POINT('Ctrl Pts',(-40.0870398284027,5.11642890754077,-0.343099580888201));
#34976=CARTESIAN_POINT('Ctrl Pts',(-39.94778118432,4.65459440947177,2.15181620303378));
#34977=CARTESIAN_POINT('Ctrl Pts',(-39.808522540237,3.0531838096976,4.11990663881172));
#34978=CARTESIAN_POINT('Ctrl Pts',(-39.6692638961543,0.704267627790603,
5.07932763235163));
#34979=CARTESIAN_POINT('Ctrl Pts',(-39.5300052520714,-1.81707314952296,
4.79518584182169));
#34980=CARTESIAN_POINT('Ctrl Pts',(-39.3907466079886,-3.89354312734584,
3.33704719832106));
#34981=CARTESIAN_POINT('Ctrl Pts',(-39.2514879639057,-5.01676384034499,
1.06190520223392));
#34982=CARTESIAN_POINT('Ctrl Pts',(-39.1122293198229,-4.91173915161331,
-1.47322116290581));
#34983=CARTESIAN_POINT('Ctrl Pts',(-38.9729706757401,-3.60418206959766,
-3.64766140116037));
#34984=CARTESIAN_POINT('Ctrl Pts',(-38.8337120316572,-1.41421947780232,
-4.92905116193056));
#34985=CARTESIAN_POINT('Ctrl Pts',(-38.6944533875743,1.12198396286053,-5.00367006060634));
#34986=CARTESIAN_POINT('Ctrl Pts',(-38.5551947434916,3.38349405796131,-3.85324928444358));
#34987=CARTESIAN_POINT('Ctrl Pts',(-38.4159360994086,4.81662929812997,-1.75944431361739));
#34988=CARTESIAN_POINT('Ctrl Pts',(-38.2766774553259,5.07051772191601,0.765122290918382));
#34989=CARTESIAN_POINT('Ctrl Pts',(-38.137418811243,4.08300027639372,3.10236536070355));
#34990=CARTESIAN_POINT('Ctrl Pts',(-37.9981601671602,2.09584910794909,4.68006181636883));
#34991=CARTESIAN_POINT('Ctrl Pts',(-37.8589015230773,-0.404425083919172,
5.11194703022454));
#34992=CARTESIAN_POINT('Ctrl Pts',(-37.7196428789945,-2.80568459910014,
4.29228331062813));
#34993=CARTESIAN_POINT('Ctrl Pts',(-37.5803842349116,-4.5200333253302,2.42174747367039));
#34994=CARTESIAN_POINT('Ctrl Pts',(-37.4411255908289,-5.12775030165407,
-0.041700506124886));
#34995=CARTESIAN_POINT('Ctrl Pts',(-37.3018669467459,-4.48004925758386,
-2.49493902489554));
#34996=CARTESIAN_POINT('Ctrl Pts',(-37.1626083026632,-2.7355056920653,-4.33734604303171));
#34997=CARTESIAN_POINT('Ctrl Pts',(-37.0233496585803,-0.321233115053798,
-5.11784831487974));
#34998=CARTESIAN_POINT('Ctrl Pts',(-36.8840910144975,2.17168639631715,-4.64535685221012));
#34999=CARTESIAN_POINT('Ctrl Pts',(-36.7448323704146,4.13291577533089,-3.03555090261152));
#35000=CARTESIAN_POINT('Ctrl Pts',(-36.6055737263318,5.08229070826373,-0.68255640427784));
#35001=CARTESIAN_POINT('Ctrl Pts',(-36.4663150822489,4.78737741250149,1.8375471690803));
#35002=CARTESIAN_POINT('Ctrl Pts',(-36.3270564381661,3.3203789876831,3.90776732501783));
#35003=CARTESIAN_POINT('Ctrl Pts',(-36.1877977940833,1.04045805875398,5.02125573101972));
#35004=CARTESIAN_POINT('Ctrl Pts',(-36.0485391500004,-1.49419637309213,
4.90539899365616));
#35005=CARTESIAN_POINT('Ctrl Pts',(-35.9092805059176,-3.66302935450954,
3.58856211264706));
#35006=CARTESIAN_POINT('Ctrl Pts',(-35.7700218618348,-4.9350493496549,1.39314392824117));
#35007=CARTESIAN_POINT('Ctrl Pts',(-35.6307632177519,-4.99882995703361,
-1.14335521557734));
#35008=CARTESIAN_POINT('Ctrl Pts',(-35.4915045736691,-3.8387558835552,-3.39992872789929));
#35009=CARTESIAN_POINT('Ctrl Pts',(-35.3522459295862,-1.73884600907171,
-4.82410371416908));
#35010=CARTESIAN_POINT('Ctrl Pts',(-35.2129872855035,0.786782452717923,
-5.06720193602146));
#35011=CARTESIAN_POINT('Ctrl Pts',(-35.0737286414205,3.11978436072366,-4.06970608655078));
#35012=CARTESIAN_POINT('Ctrl Pts',(-34.9344699973378,4.68897499169966,-2.07583130710078));
#35013=CARTESIAN_POINT('Ctrl Pts',(-34.7952113532549,5.11017218394326,0.426265573061127));
#35014=CARTESIAN_POINT('Ctrl Pts',(-34.6559527091721,4.28025497520489,2.82400060827867));
#35015=CARTESIAN_POINT('Ctrl Pts',(-34.5166940650892,2.40241052515365,4.53034057847261));
#35016=CARTESIAN_POINT('Ctrl Pts',(-34.3774354210064,-0.0636118368933031,
5.12752529223713));
#35017=CARTESIAN_POINT('Ctrl Pts',(-34.2381767769235,-2.51406022562872,
4.46934707426445));
#35018=CARTESIAN_POINT('Ctrl Pts',(-34.0989181328408,-4.34899570403538,
2.71694653142206));
#35019=CARTESIAN_POINT('Ctrl Pts',(-33.9596594887578,-5.11917427029261,
0.29936078350168));
#35020=CARTESIAN_POINT('Ctrl Pts',(-33.8204008446751,-4.63603447071792,
-2.19151693460024));
#35021=CARTESIAN_POINT('Ctrl Pts',(-33.6811422005921,-3.01786256635649,
-4.1458494447952));
#35022=CARTESIAN_POINT('Ctrl Pts',(-33.5418835565094,-0.660832717283021,
-5.08516098153175));
#35023=CARTESIAN_POINT('Ctrl Pts',(-33.4026249124265,1.85798763502059,-4.7794815656549));
#35024=CARTESIAN_POINT('Ctrl Pts',(-33.2633662683437,3.92192016684631,-3.30365014691457));
#35025=CARTESIAN_POINT('Ctrl Pts',(-33.1241076242608,5.02565593354922,-1.01899191650671));
#35026=CARTESIAN_POINT('Ctrl Pts',(-32.9848489801781,4.89896926309818,1.51514429924805));
#35027=CARTESIAN_POINT('Ctrl Pts',(-32.8455903360952,3.57287662854112,3.67833042093137));
#35028=CARTESIAN_POINT('Ctrl Pts',(-32.7063316920124,1.37204293986752,4.94095742336282));
#35029=CARTESIAN_POINT('Ctrl Pts',(-32.5670730479295,-1.16470559062442,
4.99389857481034));
#35030=CARTESIAN_POINT('Ctrl Pts',(-32.4278144038467,-3.41630131512815,
3.82419238697246));
#35031=CARTESIAN_POINT('Ctrl Pts',(-32.2885557597638,-4.8314900420594,1.71821595319255));
#35032=CARTESIAN_POINT('Ctrl Pts',(-32.149297115681,-5.06379362300385,-0.808428247867442));
#35033=CARTESIAN_POINT('Ctrl Pts',(-32.0100384715981,-4.0563375838621,-3.13714639347168));
#35034=CARTESIAN_POINT('Ctrl Pts',(-31.8707798275153,-2.05577560156633,
-4.69780254633261));
#35035=CARTESIAN_POINT('Ctrl Pts',(-31.7315211834325,0.448098278592388,
-5.10830402590205));
#35036=CARTESIAN_POINT('Ctrl Pts',(-31.5922625393496,2.84226505119731,-4.26814848231254));
#35037=CARTESIAN_POINT('Ctrl Pts',(-31.4530038952668,4.54056510758199,-2.38302970861326));
#35038=CARTESIAN_POINT('Ctrl Pts',(-31.313745251184,5.12720665419247,0.0855220061093843));
#35039=CARTESIAN_POINT('Ctrl Pts',(-31.1744866071012,4.45856328065359,2.5331355196144));
#35040=CARTESIAN_POINT('Ctrl Pts',(-31.0352279630183,2.69833775932673,4.360565952364));
#35041=CARTESIAN_POINT('Ctrl Pts',(-30.8959693189355,0.277482985620765,
5.12040674956741));
#35042=CARTESIAN_POINT('Ctrl Pts',(-30.7567106748526,-2.21130745577726,
4.62662743522194));
#35043=CARTESIAN_POINT('Ctrl Pts',(-30.6174520307698,-4.15870741103577,
3.00011912392169));
#35044=CARTESIAN_POINT('Ctrl Pts',(-30.478193386687,-5.08793839974446,0.639096963480733));
#35045=CARTESIAN_POINT('Ctrl Pts',(-30.3389347426041,-4.7714984454601,-1.87839417410094));
#35046=CARTESIAN_POINT('Ctrl Pts',(-30.1996760985213,-3.28686098148408,
-3.93600139440042));
#35047=CARTESIAN_POINT('Ctrl Pts',(-30.0604174544384,-0.997507167463827,
-5.02996436758579));
#35048=CARTESIAN_POINT('Ctrl Pts',(-29.9211588103556,1.53606455886436,-4.89245007734626));
#35049=CARTESIAN_POINT('Ctrl Pts',(-29.7819001662728,3.69356432102827,-3.55712590369689));
#35050=CARTESIAN_POINT('Ctrl Pts',(-29.6426415221899,4.94677527517285,-1.35091689798559));
#35051=CARTESIAN_POINT('Ctrl Pts',(-29.5033828781071,4.98887600398362,1.18603469814376));
#35052=CARTESIAN_POINT('Ctrl Pts',(-29.3641242340243,3.80955906062489,3.43261152068441));
#35053=CARTESIAN_POINT('Ctrl Pts',(-29.2248655899414,1.6975545226847,4.83878814692659));
#35054=CARTESIAN_POINT('Ctrl Pts',(-29.0856069458586,-0.83005928111469,
5.06029284509897));
#35055=CARTESIAN_POINT('Ctrl Pts',(-28.9463483017757,-3.15445114191686,
4.0428950124365));
#35056=CARTESIAN_POINT('Ctrl Pts',(-28.807089657693,-4.70654431907648,2.03568235756303));
#35057=CARTESIAN_POINT('Ctrl Pts',(-28.66783101361,-5.10634259021348,-0.469922801847675));
#35058=CARTESIAN_POINT('Ctrl Pts',(-28.5285723695273,-4.25596405301566,
-2.86047759434731));
#35059=CARTESIAN_POINT('Ctrl Pts',(-28.3893137254443,-2.36360537794301,
-4.55070672595844));
#35060=CARTESIAN_POINT('Ctrl Pts',(-28.2500550813616,0.107430613693398,
-5.12679439333839));
#35061=CARTESIAN_POINT('Ctrl Pts',(-28.1107964372787,2.55216455853763,-4.44769807366338));
#35062=CARTESIAN_POINT('Ctrl Pts',(-27.9715377931959,4.37205657674479,-2.67967971557556));
#35063=CARTESIAN_POINT('Ctrl Pts',(-27.832279149113,5.12154573019909,-0.255600120899675));
#35064=CARTESIAN_POINT('Ctrl Pts',(-27.6930205050302,4.61713591749465,2.23105759847328));
#35065=CARTESIAN_POINT('Ctrl Pts',(-27.5537618609474,2.98232089930236,4.17148943926614));
#35066=CARTESIAN_POINT('Ctrl Pts',(-27.4145032168645,0.617349539765915,
5.09062291218622));
#35067=CARTESIAN_POINT('Ctrl Pts',(-27.2752445727817,-1.89876641369781,
4.76342819768889));
#35068=CARTESIAN_POINT('Ctrl Pts',(-27.1359859286988,-3.9500107505568,3.27001179796192));
#35069=CARTESIAN_POINT('Ctrl Pts',(-26.996727284616,-5.03418095445742,0.97600420393705));
#35070=CARTESIAN_POINT('Ctrl Pts',(-26.8574686405332,-4.88584155544076,
-1.55695676993701));
#35071=CARTESIAN_POINT('Ctrl Pts',(-26.7182099964503,-3.54131022572266,
-3.7087307766292));
#35072=CARTESIAN_POINT('Ctrl Pts',(-26.5789513523675,-1.32976618835693,
-4.95250279885102));
#35073=CARTESIAN_POINT('Ctrl Pts',(-26.4396927082847,1.20734214866586,-4.9837623362656));
#35074=CARTESIAN_POINT('Ctrl Pts',(-26.3004340642018,3.44885904674366,-3.79485617171704));
#35075=CARTESIAN_POINT('Ctrl Pts',(-26.161175420119,4.84599789550719,-1.67686209482602));
#35076=CARTESIAN_POINT('Ctrl Pts',(-26.0219167760362,5.05669966623105,0.851675157476819));
#35077=CARTESIAN_POINT('Ctrl Pts',(-25.8826581319533,4.02937861773551,3.1716982900743));
#35078=CARTESIAN_POINT('Ctrl Pts',(-25.7433994878705,2.01555194199366,4.71520015030647));
#35079=CARTESIAN_POINT('Ctrl Pts',(-25.6041408437876,-0.491738744311117,
5.1042879126934));
#35080=CARTESIAN_POINT('Ctrl Pts',(-25.4648821997048,-2.87863790516758,
4.24370190980198));
#35081=CARTESIAN_POINT('Ctrl Pts',(-25.325623555622,-4.56076524841596,2.3441378878312));
#35082=CARTESIAN_POINT('Ctrl Pts',(-25.1863649115391,-5.12628851720279,
-0.129337259594039));
#35083=CARTESIAN_POINT('Ctrl Pts',(-25.0471062674563,-4.43675165169258,
-2.57114699492807));
#35084=CARTESIAN_POINT('Ctrl Pts',(-24.9078476233734,-2.6609727408645,-4.38346736735891));
#35085=CARTESIAN_POINT('Ctrl Pts',(-24.7685889792906,-0.233712588919614,
-5.12259119138986));
#35086=CARTESIAN_POINT('Ctrl Pts',(-24.6293303352077,2.25076700205062,-4.60756009085119));
#35087=CARTESIAN_POINT('Ctrl Pts',(-24.490071691125,4.18419529608634,-2.96446821749421));
#35088=CARTESIAN_POINT('Ctrl Pts',(-24.3508130470421,5.09321446983781,-0.595590843246681));
#35089=CARTESIAN_POINT('Ctrl Pts',(-24.2115544029592,4.75527096970404,1.91910398181406));
#35090=CARTESIAN_POINT('Ctrl Pts',(-24.0722957588764,3.25310290401414,3.96394797950469));
#35091=CARTESIAN_POINT('Ctrl Pts',(-23.9330371147936,0.954483418570409,
5.03830561716918));
#35092=CARTESIAN_POINT('Ctrl Pts',(-23.7937784707108,-1.57782055097424,
4.8791438180533));
#35093=CARTESIAN_POINT('Ctrl Pts',(-23.6545198266279,-3.72382951079462,
3.52542988341273));
#35094=CARTESIAN_POINT('Ctrl Pts',(-23.5152611825451,-4.95813988981271,
1.30859119719357));
#35095=CARTESIAN_POINT('Ctrl Pts',(-23.3760025384622,-4.97855766503187,
-1.22862755311651));
#35096=CARTESIAN_POINT('Ctrl Pts',(-23.2367438943794,-3.78008398872379,
-3.46504359662597));
#35097=CARTESIAN_POINT('Ctrl Pts',(-23.0974852502966,-1.65613904746037,
-4.85311915615117));
#35098=CARTESIAN_POINT('Ctrl Pts',(-22.9582266062137,0.873275482247959,
-5.05301415201156));
#35099=CARTESIAN_POINT('Ctrl Pts',(-22.8189679621309,3.18888752301124,-4.01578864656841));
#35100=CARTESIAN_POINT('Ctrl Pts',(-22.679709318048,4.72376988196712,-1.99538472243945));
#35101=CARTESIAN_POINT('Ctrl Pts',(-22.5404506739652,5.10214003086018,0.513545707623582));
#35102=CARTESIAN_POINT('Ctrl Pts',(-22.4011920298823,4.23136227657829,2.89674565205072));
#35103=CARTESIAN_POINT('Ctrl Pts',(-22.2619333857996,2.32462759375435,4.57074049128587));
#35104=CARTESIAN_POINT('Ctrl Pts',(-22.1226747417167,-0.151241543795875,
5.12568903502298));
#35105=CARTESIAN_POINT('Ctrl Pts',(-21.9834160976339,-2.59008248216644,
4.42572421462287));
#35106=CARTESIAN_POINT('Ctrl Pts',(-21.844157453551,-4.39479811584537,2.64221717678288));
#35107=CARTESIAN_POINT('Ctrl Pts',(-21.7048988094682,-5.12354311404958,
0.211820789346871));
#35108=CARTESIAN_POINT('Ctrl Pts',(-21.5656401653853,-4.59790013014616,
-2.27043530661552));
#35109=CARTESIAN_POINT('Ctrl Pts',(-21.4263815213025,-2.94656140448722,
-4.19682474948749));
#35110=CARTESIAN_POINT('Ctrl Pts',(-21.2871228772196,-0.573821271236779,
-5.09571302537738));
#35111=CARTESIAN_POINT('Ctrl Pts',(-21.1478642331369,1.93940650708562,-4.74702691045655));
#35112=CARTESIAN_POINT('Ctrl Pts',(-21.008605589054,3.97781282675011,-3.23613460839731));
#35113=CARTESIAN_POINT('Ctrl Pts',(-20.8693469449712,5.04233828040476,-0.932945204333682));
#35114=CARTESIAN_POINT('Ctrl Pts',(-20.7300883008883,4.87235698748461,1.59865552100332));
#35115=CARTESIAN_POINT('Ctrl Pts',(-20.5908296568055,3.50948516674211,3.73886024782176));
#35116=CARTESIAN_POINT('Ctrl Pts',(-20.4515710127226,1.28739231115071,4.96368644512469));
#35117=CARTESIAN_POINT('Ctrl Pts',(-20.3123123686398,-1.24989052282436,
4.97326208531968));
#35118=CARTESIAN_POINT('Ctrl Pts',(-20.173053724557,-3.48116487480147,3.76524278138513));
#35119=CARTESIAN_POINT('Ctrl Pts',(-20.0337950804741,-4.86015179882432,
1.63538575899058));
#35120=CARTESIAN_POINT('Ctrl Pts',(-19.8945364363913,-5.04923636973798,
-0.894859861006039));
#35121=CARTESIAN_POINT('Ctrl Pts',(-19.7552777923085,-4.00212534708821,
-3.20601852685208));
#35122=CARTESIAN_POINT('Ctrl Pts',(-19.6160191482256,-1.97518106715403,
-4.7322533575751));
#35123=CARTESIAN_POINT('Ctrl Pts',(-19.4767605041428,0.535343293589886,
-5.09989898393416));
#35124=CARTESIAN_POINT('Ctrl Pts',(-19.3375018600599,2.91480050434934,-4.21894537866626));
#35125=CARTESIAN_POINT('Ctrl Pts',(-19.1982432159771,4.5806322724203,-2.30507485197035));
#35126=CARTESIAN_POINT('Ctrl Pts',(-19.0589845718943,5.12499595774547,0.17314306632675));
#35127=CARTESIAN_POINT('Ctrl Pts',(-18.9197259278114,4.41461596381525,2.60897067449063));
#35128=CARTESIAN_POINT('Ctrl Pts',(-18.7804672837286,2.6234133658075,4.40604861530454));
#35129=CARTESIAN_POINT('Ctrl Pts',(-18.6412086396458,0.189925121925963,
5.12440148079616));
#35130=CARTESIAN_POINT('Ctrl Pts',(-18.5019499955629,-2.29006215302471,
4.58815621177052));
#35131=CARTESIAN_POINT('Ctrl Pts',(-18.3626913514801,-4.20937756885579,
2.92860078725975));
#35132=CARTESIAN_POINT('Ctrl Pts',(-18.2234327073973,-5.09811853318134,
0.552041221248485));
#35133=CARTESIAN_POINT('Ctrl Pts',(-18.0841740633144,-4.73869617048286,
-1.95967361878847));
#35134=CARTESIAN_POINT('Ctrl Pts',(-17.9449154192316,-3.21910722095246,
-3.99160503912099));
#35135=CARTESIAN_POINT('Ctrl Pts',(-17.8056567751488,-0.911389954514629,
-5.04627887052769));
#35136=CARTESIAN_POINT('Ctrl Pts',(-17.6663981310659,1.61946129957759,-4.86548118766222));
#35137=CARTESIAN_POINT('Ctrl Pts',(-17.5271394869831,3.75382271324905,-3.49347636686155));
#35138=CARTESIAN_POINT('Ctrl Pts',(-17.3878808429002,4.96914236350674,-1.26616991732043));
#35139=CARTESIAN_POINT('Ctrl Pts',(-17.2486221988174,4.96787569382644,1.27113066952724));
#35140=CARTESIAN_POINT('Ctrl Pts',(-17.1093635547345,3.75033282070164,3.49722258689558));
#35141=CARTESIAN_POINT('Ctrl Pts',(-16.9701049106517,1.61460260837161,4.86709569511061));
#35142=CARTESIAN_POINT('Ctrl Pts',(-16.8308462665689,-0.916427899620469,
5.0453663883926));
#35143=CARTESIAN_POINT('Ctrl Pts',(-16.691587622486,-3.22309098878473,3.98838896878665));
#35144=CARTESIAN_POINT('Ctrl Pts',(-16.5523289784032,-4.74065042222205,
1.95494134505625));
#35145=CARTESIAN_POINT('Ctrl Pts',(-16.4130703343204,-5.09756481283691,
-0.557131104185897));
#35146=CARTESIAN_POINT('Ctrl Pts',(-16.2738116902375,-4.20645144279858,
-2.93280213238163));
#35147=CARTESIAN_POINT('Ctrl Pts',(-16.1345530461547,-2.28548001951246,
-4.5904404111952));
#35148=CARTESIAN_POINT('Ctrl Pts',(-15.9952944020718,0.195041427264702,
-5.1242092980259));
#35149=CARTESIAN_POINT('Ctrl Pts',(-15.856035757989,2.62781122700226,-4.40342710210641));
#35150=CARTESIAN_POINT('Ctrl Pts',(-15.7167771139062,4.41721866030238,-2.60456165129585));
#35151=CARTESIAN_POINT('Ctrl Pts',(-15.5775184698233,5.12516627595581,-0.16802598647164));
#35152=CARTESIAN_POINT('Ctrl Pts',(-15.4382598257405,4.57832851364817,2.30964718289191));
#35153=CARTESIAN_POINT('Ctrl Pts',(-15.2990011816576,2.91058669377287,4.22185352497654));
#35154=CARTESIAN_POINT('Ctrl Pts',(-15.1597425375748,0.530251090985978,
5.10043094932504));
#35155=CARTESIAN_POINT('Ctrl Pts',(-15.020483893492,-1.97990494684484,4.73027890190248));
#35156=CARTESIAN_POINT('Ctrl Pts',(-14.8812252494091,-4.00532436477151,
3.20202105259979));
#35157=CARTESIAN_POINT('Ctrl Pts',(-14.7419666053263,-5.05012731558285,
0.889818062712039));
#35158=CARTESIAN_POINT('Ctrl Pts',(-14.6027079612435,-4.8585165441382,-1.64023750678368));
#35159=CARTESIAN_POINT('Ctrl Pts',(-14.4634493171606,-3.47740377609158,
-3.76871663386205));
#35160=CARTESIAN_POINT('Ctrl Pts',(-14.3241906730778,-1.2449244032235,-4.9745075453338));
#35161=CARTESIAN_POINT('Ctrl Pts',(-14.184932028995,1.29234760538017,-4.96239858890765));
#35162=CARTESIAN_POINT('Ctrl Pts',(-14.0456733849121,3.51321643969437,-3.73535437892922));
#35163=CARTESIAN_POINT('Ctrl Pts',(-13.9064147408293,4.87395071821435,-1.59378997510416));
#35164=CARTESIAN_POINT('Ctrl Pts',(-13.7671560967465,5.04140427864135,0.937979204258423));
#35165=CARTESIAN_POINT('Ctrl Pts',(-13.6278974526636,3.97457976249027,3.24010459706584));
#35166=CARTESIAN_POINT('Ctrl Pts',(-13.4886388085808,1.93466592572345,4.74896092257761));
#35167=CARTESIAN_POINT('Ctrl Pts',(-13.3493801644979,-0.57890874156636,
5.09513756019038));
#35168=CARTESIAN_POINT('Ctrl Pts',(-13.2101215204151,-2.95075020743805,
4.1938806971144));
#35169=CARTESIAN_POINT('Ctrl Pts',(-13.0708628763322,-4.60016472851397,
2.26584345418221));
#35170=CARTESIAN_POINT('Ctrl Pts',(-12.9316042322494,-5.12332907022864,
-0.216936226745527));
#35171=CARTESIAN_POINT('Ctrl Pts',(-12.7923455881666,-4.39215783380509,
-2.64660379567266));
#35172=CARTESIAN_POINT('Ctrl Pts',(-12.6530869440837,-2.58566237748044,
-4.42830804687374));
#35173=CARTESIAN_POINT('Ctrl Pts',(-12.5138283000009,-0.146123782862334,
-5.12583748556338));
#35174=CARTESIAN_POINT('Ctrl Pts',(-12.3745696559181,2.3291900385944,-4.56841721523299));
#35175=CARTESIAN_POINT('Ctrl Pts',(-12.2353110118352,4.23425239003886,-2.8925194529639));
#35176=CARTESIAN_POINT('Ctrl Pts',(-12.0960523677524,5.1026502315838,-0.50845127833681));
#35177=CARTESIAN_POINT('Ctrl Pts',(-11.9567937236695,4.72177525841466,2.00010012183084));
#35178=CARTESIAN_POINT('Ctrl Pts',(-11.8175350795867,3.18487641533271,4.01897055318671));
#35179=CARTESIAN_POINT('Ctrl Pts',(-11.6782764355039,0.868229922828961,
5.05388354529751));
#35180=CARTESIAN_POINT('Ctrl Pts',(-11.539017791421,-1.66098376324763,4.85146318408707));
#35181=CARTESIAN_POINT('Ctrl Pts',(-11.3997591473382,-3.78354173769753,
3.461267687918));
#35182=CARTESIAN_POINT('Ctrl Pts',(-11.2605005032553,-4.97978189263771,
1.2236561568031));
#35183=CARTESIAN_POINT('Ctrl Pts',(-11.1212418591726,-4.9568308705752,-1.31354094296196));
#35184=CARTESIAN_POINT('Ctrl Pts',(-10.9819832150897,-3.72030772957414,
-3.52914614115021));
#35185=CARTESIAN_POINT('Ctrl Pts',(-10.8427245710069,-1.57294823922665,
-4.88071674296288));
#35186=CARTESIAN_POINT('Ctrl Pts',(-10.703465926924,0.959513381393236,-5.03735011283231));
#35187=CARTESIAN_POINT('Ctrl Pts',(-10.5642072828412,3.25705904102695,-3.96069798035511));
#35188=CARTESIAN_POINT('Ctrl Pts',(-10.4249486387583,4.75718470689197,-1.91435517938488));
#35189=CARTESIAN_POINT('Ctrl Pts',(-10.2856899946755,5.09261727031618,0.60067580807126));
#35190=CARTESIAN_POINT('Ctrl Pts',(-10.1464313505927,4.18123337115581,2.96864440178638));
#35191=CARTESIAN_POINT('Ctrl Pts',(-10.0071727065098,2.24616551454361,4.60980504681049));
#35192=CARTESIAN_POINT('Ctrl Pts',(-9.86791406242699,-0.238827064970182,
5.12235529042668));
#35193=CARTESIAN_POINT('Ctrl Pts',(-9.72865541834415,-2.66534803734968,
4.38080836468806));
#35194=CARTESIAN_POINT('Ctrl Pts',(-9.58939677426131,-4.43931657252653,
2.56671588946183));
#35195=CARTESIAN_POINT('Ctrl Pts',(-9.45013813017847,-5.12641509736252,
0.124218911032201));
#35196=CARTESIAN_POINT('Ctrl Pts',(-9.31087948609565,-4.55842249750529,
-2.3486903632795));
#35197=CARTESIAN_POINT('Ctrl Pts',(-9.1716208420128,-2.87439939474084,-4.24657393763936));
#35198=CARTESIAN_POINT('Ctrl Pts',(-9.03236219792996,-0.486642181365819,
-5.1047763394335));
#35199=CARTESIAN_POINT('Ctrl Pts',(-8.89310355384714,2.02025877498237,-4.71318539529599));
#35200=CARTESIAN_POINT('Ctrl Pts',(-8.75384490976428,4.03254335518717,-3.16767362221242));
#35201=CARTESIAN_POINT('Ctrl Pts',(-8.61458626568145,5.05754749108297,-0.846625929064747));
#35202=CARTESIAN_POINT('Ctrl Pts',(-8.47532762159861,4.84432123630313,1.681699690143));
#35203=CARTESIAN_POINT('Ctrl Pts',(-8.33606897751578,3.44506839698563,3.79829775404922));
#35204=CARTESIAN_POINT('Ctrl Pts',(-8.19681033343293,1.20236556641743,4.98496530910879));
#35205=CARTESIAN_POINT('Ctrl Pts',(-8.0575516893501,-1.33471029528195,4.95117264049567));
#35206=CARTESIAN_POINT('Ctrl Pts',(-7.91829304526727,-3.54501140038643,
3.70519314738851));
#35207=CARTESIAN_POINT('Ctrl Pts',(-7.77903440118442,-4.88739364580853,
1.55207778130958));
#35208=CARTESIAN_POINT('Ctrl Pts',(-7.63977575710159,-5.03320396499462,
-0.98103003781074));
#35209=CARTESIAN_POINT('Ctrl Pts',(-7.50051711301875,-3.94674387586246,
-3.27395401108));
#35210=CARTESIAN_POINT('Ctrl Pts',(-7.36125846893591,-1.89400947691462,
-4.7653216249989));
#35211=CARTESIAN_POINT('Ctrl Pts',(-7.22199982485306,0.622431906234182,
-5.09000398923479));
#35212=CARTESIAN_POINT('Ctrl Pts',(-7.08274118077025,2.98648438867875,-4.16850969586284));
#35213=CARTESIAN_POINT('Ctrl Pts',(-6.94348253668739,4.61936119005255,-2.22644655991574));
#35214=CARTESIAN_POINT('Ctrl Pts',(-6.80422389260458,5.12128797640124,0.260713542211845));
#35215=CARTESIAN_POINT('Ctrl Pts',(-6.66496524852172,4.36937890199675,2.68404360976314));
#35216=CARTESIAN_POINT('Ctrl Pts',(-6.52570660443889,2.54772253320329,4.45024403624483));
#35217=CARTESIAN_POINT('Ctrl Pts',(-6.38644796035604,0.102311770964511,
5.12689910080611));
#35218=CARTESIAN_POINT('Ctrl Pts',(-6.24718931627322,-2.3681478008713,4.54834454296868));
#35219=CARTESIAN_POINT('Ctrl Pts',(-6.10793067219037,-4.25881794278671,
2.85622684997581));
#35220=CARTESIAN_POINT('Ctrl Pts',(-5.96867202810753,-5.10680923405142,
0.464824198306887));
#35221=CARTESIAN_POINT('Ctrl Pts',(-5.82941338402469,-4.70450946939732,
-2.04038053820247));
#35222=CARTESIAN_POINT('Ctrl Pts',(-5.69015473994187,-3.150412987362,-4.0460425229334));
#35223=CARTESIAN_POINT('Ctrl Pts',(-5.55089609585902,-0.825006475908536,
-5.06111908603556));
#35224=CARTESIAN_POINT('Ctrl Pts',(-5.41163745177619,1.70238490919671,-4.83709083119842));
#35225=CARTESIAN_POINT('Ctrl Pts',(-5.27237880769335,3.81298441347213,-3.42880619909369));
#35226=CARTESIAN_POINT('Ctrl Pts',(-5.13312016361051,4.99005770009789,-1.18105302083279));
#35227=CARTESIAN_POINT('Ctrl Pts',(-4.99386151952767,4.94542400198837,1.35585527578786));
#35228=CARTESIAN_POINT('Ctrl Pts',(-4.85460287544484,3.69001090836444,3.56081192770356));
#35229=CARTESIAN_POINT('Ctrl Pts',(-4.715344231362,1.53117898244731,4.89398130483108));
#35230=CARTESIAN_POINT('Ctrl Pts',(-4.57608558727916,-1.00252878061676,
5.0289659108369));
#35231=CARTESIAN_POINT('Ctrl Pts',(-4.43682694319632,-3.29078919872254,
3.93271770381442));
#35232=CARTESIAN_POINT('Ctrl Pts',(-4.29756829911349,-4.77337152831812,
1.87362918982565));
#35233=CARTESIAN_POINT('Ctrl Pts',(-4.15830965503064,-5.08729776466478,
-0.644176638788498));
#35234=CARTESIAN_POINT('Ctrl Pts',(-4.01905101094782,-4.15570990356999,
-3.0042698423568));
#35235=CARTESIAN_POINT('Ctrl Pts',(-3.87979236686497,-2.20668695036655,
-4.62883298374532));
#35236=CARTESIAN_POINT('Ctrl Pts',(-3.74053372278213,0.28259525882338,-5.12012714764091));
#35237=CARTESIAN_POINT('Ctrl Pts',(-3.60127507869929,2.70269017153252,-4.35786965443408));
#35238=CARTESIAN_POINT('Ctrl Pts',(-3.46201643461646,4.46109023849236,-2.52868265552132));
#35239=CARTESIAN_POINT('Ctrl Pts',(-3.32275779053363,5.12728948705797,-0.0804027626875136));
#35240=CARTESIAN_POINT('Ctrl Pts',(-3.18349914645079,4.53818353564321,2.38756199608455));
#35241=CARTESIAN_POINT('Ctrl Pts',(-3.04424050236796,2.83800215050638,4.27098418189009));
#35242=CARTESIAN_POINT('Ctrl Pts',(-2.90498185828511,0.442997727543895,
5.10874887834615));
#35243=CARTESIAN_POINT('Ctrl Pts',(-2.76572321420227,-2.06046504404221,
4.69574763908411));
#35244=CARTESIAN_POINT('Ctrl Pts',(-2.62646457011944,-4.05946780997995,
3.13309482607209));
#35245=CARTESIAN_POINT('Ctrl Pts',(-2.48720592603659,-5.06459826484176,
0.803371957913989));
#35246=CARTESIAN_POINT('Ctrl Pts',(-2.34794728195375,-4.8297721009878,-1.72303904227276));
#35247=CARTESIAN_POINT('Ctrl Pts',(-2.20868863787092,-3.41248139082355,
-3.82760144861539));
#35248=CARTESIAN_POINT('Ctrl Pts',(-2.06942999378809,-1.15971890993101,
-4.99505897100328));
#35249=CARTESIAN_POINT('Ctrl Pts',(-1.93017134970524,1.37697549976642,-4.93958506317368));
#35250=CARTESIAN_POINT('Ctrl Pts',(-1.79091270562242,3.57654743186344,-3.67476128358358));
#35251=CARTESIAN_POINT('Ctrl Pts',(-1.65165406153958,4.90047960504737,-1.51025223624387));
#35252=CARTESIAN_POINT('Ctrl Pts',(-1.51239541745672,5.02463601739066,1.02400924064084));
#35253=CARTESIAN_POINT('Ctrl Pts',(-1.3731367733739,3.91861974053298,3.3075642508956));
#35254=CARTESIAN_POINT('Ctrl Pts',(-1.23387812929106,1.85321465084221,4.7813343589219));
#35255=CARTESIAN_POINT('Ctrl Pts',(-1.09461948520821,-0.665909531765221,
5.08449847225302));
#35256=CARTESIAN_POINT('Ctrl Pts',(-0.955360841125384,-3.0220005881154,
4.1428345670361));
#35257=CARTESIAN_POINT('Ctrl Pts',(-0.816102197042551,-4.63821996216164,
2.186886385227));
#35258=CARTESIAN_POINT('Ctrl Pts',(-0.676843552959707,-5.11887339656061,
-0.30447052465205));
#35259=CARTESIAN_POINT('Ctrl Pts',(-0.537584908876869,-4.34627971767338,
-2.721289900206));
#35260=CARTESIAN_POINT('Ctrl Pts',(-0.398326264794041,-2.50959877852527,
-4.47185006834336));
#35261=CARTESIAN_POINT('Ctrl Pts',(-0.259067620711191,-0.0584880437401866,
-5.12759583452146));
#35262=CARTESIAN_POINT('Ctrl Pts',(-0.119808976628352,2.40692431658313,
-4.52792095714916));
#35263=CARTESIAN_POINT('Ctrl Pts',(0.0194496674544802,4.28308858749807,
-2.81976214164628));
#35264=CARTESIAN_POINT('Ctrl Pts',(0.158708311537312,5.11056367501673,-0.421091719996148));
#35265=CARTESIAN_POINT('Ctrl Pts',(0.297966955620156,4.68696209505367,2.08037032858027));
#35266=CARTESIAN_POINT('Ctrl Pts',(0.437225599702985,3.11559368557815,4.07311831939771));
#35267=CARTESIAN_POINT('Ctrl Pts',(0.53006469575821,1.55987615590447,4.73580748738429));
#35268=CARTESIAN_POINT('Ctrl Pts',(0.576484243785824,0.749759770534598,
4.86076571632371));
#35269=CARTESIAN_POINT('',(-8.88178419700125E-15,0.901975524284047,5.84759529345974));
#35270=CARTESIAN_POINT('Ctrl Pts',(-1.90958360235527E-14,3.90948457664364,
-2.98454410297303));
#35271=CARTESIAN_POINT('Ctrl Pts',(-1.91833507282437E-14,3.98829243888861,
-2.90007919033881));
#35272=CARTESIAN_POINT('Ctrl Pts',(-3.73580879594742E-14,4.06399823051801,
-2.81291231202011));
#35273=CARTESIAN_POINT('Ctrl Pts',(-3.49720252756924E-14,4.13644712233781,
-2.72320270054994));
#35274=CARTESIAN_POINT('Ctrl Pts',(-3.18638451300726E-14,4.22735285500253,
-2.61063896419842));
#35275=CARTESIAN_POINT('Ctrl Pts',(-1.94635529727361E-14,4.3131323964303,
-2.49407313917698));
#35276=CARTESIAN_POINT('Ctrl Pts',(-1.43218770176645E-14,4.39368586403212,
-2.37393105053264));
#35277=CARTESIAN_POINT('Ctrl Pts',(-1.10162867186718E-14,4.44547379531786,
-2.29669154221012));
#35278=CARTESIAN_POINT('Ctrl Pts',(-5.24917652412265E-15,4.4951010825493,
-2.21797295530272));
#35279=CARTESIAN_POINT('Ctrl Pts',(-3.44169137633799E-15,4.54253384538222,
-2.13787989953547));
#35280=CARTESIAN_POINT('Ctrl Pts',(-2.4768234675261E-15,4.5678543027812,
-2.09512479345715));
#35281=CARTESIAN_POINT('Ctrl Pts',(-9.30961986510496E-15,4.5925493020505,
-2.05197791192938));
#35282=CARTESIAN_POINT('Ctrl Pts',(-9.2148511043888E-15,4.61661294342695,
-2.00845450824052));
#35283=CARTESIAN_POINT('Ctrl Pts',(-9.15701027903361E-15,4.63129985995668,
-1.98189059020882));
#35284=CARTESIAN_POINT('Ctrl Pts',(-2.21079829589896E-14,4.645751578647,
-1.95518640516938));
#35285=CARTESIAN_POINT('Ctrl Pts',(-2.20934381900406E-14,4.6599666572219,
-1.92834534623301));
#35286=CARTESIAN_POINT('Ctrl Pts',(-2.20822060839698E-14,4.67094416198108,
-1.90761750778575));
#35287=CARTESIAN_POINT('Ctrl Pts',(-1.77421344277379E-14,4.68177804862746,
-1.88681267103478));
#35288=CARTESIAN_POINT('Ctrl Pts',(-1.75415237890775E-14,4.69246422230885,
-1.8659397413347));
#35289=CARTESIAN_POINT('Ctrl Pts',(-1.62668284098313E-14,4.76036498920956,
-1.73331154565338));
#35290=CARTESIAN_POINT('Ctrl Pts',(-3.47731085017832E-15,4.82235112178215,
-1.59785024042009));
#35291=CARTESIAN_POINT('Ctrl Pts',(-4.49640324973188E-15,4.87831618402814,
-1.46000130615661));
#35292=CARTESIAN_POINT('Ctrl Pts',(-5.52168602536538E-15,4.93462120051458,
-1.32131502216344));
#35293=CARTESIAN_POINT('Ctrl Pts',(-1.64490113575227E-14,4.98483221912858,
-1.18021136659838));
#35294=CARTESIAN_POINT('Ctrl Pts',(-2.18158824338843E-14,5.02880142240401,
-1.03710876150088));
#35295=CARTESIAN_POINT('Ctrl Pts',(-2.55685228577448E-14,5.05954570660026,
-0.937048109212461));
#35296=CARTESIAN_POINT('Ctrl Pts',(-6.915413085807E-15,5.08723747133457,
-0.836009395806493));
#35297=CARTESIAN_POINT('Ctrl Pts',(-7.43849426498855E-15,5.11181306297585,
-0.73412814542384));
#35298=CARTESIAN_POINT('Ctrl Pts',(-7.54805533896459E-15,5.1169605015016,
-0.712788782330314));
#35299=CARTESIAN_POINT('Ctrl Pts',(-1.50603780235338E-14,5.12197119102857,
-0.691412439291222));
#35300=CARTESIAN_POINT('Ctrl Pts',(-1.53765888910584E-14,5.12684448137593,
-0.670000335987038));
#35301=CARTESIAN_POINT('Ctrl Pts',(-1.57085190484981E-14,5.13196002988606,
-0.647523806712406));
#35302=CARTESIAN_POINT('Ctrl Pts',(-1.68377511556197E-14,5.13692242704591,
-0.62501543339186));
#35303=CARTESIAN_POINT('Ctrl Pts',(-1.62647673107585E-14,5.14172987403327,
-0.602483352090299));
#35304=CARTESIAN_POINT('Ctrl Pts',(-1.47775349171851E-14,5.15420804589469,
-0.543999257805867));
#35305=CARTESIAN_POINT('Ctrl Pts',(-2.94588731295145E-14,5.16564553352701,
-0.485341644951264));
#35306=CARTESIAN_POINT('Ctrl Pts',(-2.86992651865603E-14,5.1760363559108,
-0.426537904798046));
#35307=CARTESIAN_POINT('Ctrl Pts',(-2.68071769236455E-14,5.20198688412704,
-0.279678680214664));
#35308=CARTESIAN_POINT('Ctrl Pts',(-5.56602536354946E-15,5.22141246689856,
-0.131909892996859));
#35309=CARTESIAN_POINT('Ctrl Pts',(-7.71605002114484E-15,5.23446159560053,
0.0163413505315488));
#35310=CARTESIAN_POINT('Ctrl Pts',(-9.89977148514226E-15,5.24771524007957,
0.166916099250649));
#35311=CARTESIAN_POINT('Ctrl Pts',(-2.15550044527619E-14,5.25439114187506,
0.317989193576075));
#35312=CARTESIAN_POINT('Ctrl Pts',(-2.54796184151473E-14,5.25459601396279,
0.469135904779127));
#35313=CARTESIAN_POINT('Ctrl Pts',(-2.94411969011659E-14,5.25480281566683,
0.621706212349075));
#35314=CARTESIAN_POINT('Ctrl Pts',(-1.52795916454729E-14,5.24841622956477,
0.77435226947332));
#35315=CARTESIAN_POINT('Ctrl Pts',(-1.55986334959834E-14,5.23549467657462,
0.926649684258014));
#35316=CARTESIAN_POINT('Ctrl Pts',(-1.58261930992363E-14,5.2262782572643,
1.03527724904109));
#35317=CARTESIAN_POINT('Ctrl Pts',(-5.48374672990966E-15,5.21373617382266,
1.14372773684654));
#35318=CARTESIAN_POINT('Ctrl Pts',(-3.71924713249427E-15,5.19787343757021,
1.25184773611315));
#35319=CARTESIAN_POINT('Ctrl Pts',(-3.19499098604058E-15,5.19316040901973,
1.28397161659072));
#35320=CARTESIAN_POINT('Ctrl Pts',(-1.90671538789874E-14,5.18815415473348,
1.31606631618875));
#35321=CARTESIAN_POINT('Ctrl Pts',(-1.9373391779709E-14,5.1828545750351,
1.34812778544358));
#35322=CARTESIAN_POINT('Ctrl Pts',(-1.95571813998463E-14,5.17967401594245,
1.36736957505062));
#35323=CARTESIAN_POINT('Ctrl Pts',(-1.37749350569938E-14,5.17638788963684,
1.38659858233887));
#35324=CARTESIAN_POINT('Ctrl Pts',(-1.38777878078145E-14,5.17299861538347,
1.40580097511783));
#35325=CARTESIAN_POINT('Ctrl Pts',(-1.47043682530614E-14,5.14576057071216,
1.56012180996567));
#35326=CARTESIAN_POINT('Ctrl Pts',(-7.96362220616864E-15,5.11182907899611,
1.71294254845863));
#35327=CARTESIAN_POINT('Ctrl Pts',(-1.03805852802452E-14,5.07133602327383,
1.86381417395566));
#35328=CARTESIAN_POINT('Ctrl Pts',(-1.22216136978406E-14,5.0404919995899,
1.97873481669447));
#35329=CARTESIAN_POINT('Ctrl Pts',(-1.14125186604969E-14,5.00583989091105,
2.09252508158171));
#35330=CARTESIAN_POINT('Ctrl Pts',(-9.88098491916389E-15,4.96741807624543,
2.20499024943516));
#35331=CARTESIAN_POINT('Ctrl Pts',(-7.88224225419095E-15,4.9172753218514,
2.35176398562226));
#35332=CARTESIAN_POINT('Ctrl Pts',(-1.31674334524512E-15,4.86071404285811,
2.49628151547096));
#35333=CARTESIAN_POINT('Ctrl Pts',(-1.4432899320127E-15,4.79803186865836,
2.63821945379872));
#35334=CARTESIAN_POINT('Ctrl Pts',(-1.57089238570486E-15,4.73482669311825,
2.78134167989155));
#35335=CARTESIAN_POINT('Ctrl Pts',(-9.37532187212029E-16,4.665397799525,
2.92184176943859));
#35336=CARTESIAN_POINT('Ctrl Pts',(-2.66453525910038E-15,4.58999880867953,
3.05937585270003));
#35337=CARTESIAN_POINT('Ctrl Pts',(-3.51498131210545E-15,4.55286930080032,
3.12710318924464));
#35338=CARTESIAN_POINT('Ctrl Pts',(-1.51993577605973E-14,4.51429129789493,
3.19411102466394));
#35339=CARTESIAN_POINT('Ctrl Pts',(-1.48214773787458E-14,4.47429084970801,
3.26035642397394));
#35340=CARTESIAN_POINT('Ctrl Pts',(-1.46923288761638E-14,4.46061986218376,
3.28299717097943));
#35341=CARTESIAN_POINT('Ctrl Pts',(-3.01425676435767E-14,4.44678269964352,
3.3055488470762));
#35342=CARTESIAN_POINT('Ctrl Pts',(-3.05866443284231E-14,4.43278033145175,
3.32800969615114));
#35343=CARTESIAN_POINT('Ctrl Pts',(-3.09193787759791E-14,4.42228874203993,
3.34483899267496));
#35344=CARTESIAN_POINT('Ctrl Pts',(-1.22788573377448E-14,4.41170953178767,
3.36160906394854));
#35345=CARTESIAN_POINT('Ctrl Pts',(-1.22957199977236E-14,4.40104403199575,
3.37831829577569));
#35346=CARTESIAN_POINT('Ctrl Pts',(-1.24315705710625E-14,4.31511961298378,
3.51293280657181));
#35347=CARTESIAN_POINT('Ctrl Pts',(-6.54470196245199E-15,4.22358573877092,
3.64362044463653));
#35348=CARTESIAN_POINT('Ctrl Pts',(-9.29811783123569E-15,4.12678394837992,
3.7700546431706));
#35349=CARTESIAN_POINT('Ctrl Pts',(-1.21936673961834E-14,4.02498516628143,
3.90301548381599));
#35350=CARTESIAN_POINT('Ctrl Pts',(-1.35210479601085E-15,3.91736062357425,
4.031273317785));
#35351=CARTESIAN_POINT('Ctrl Pts',(-3.83026943495679E-15,3.80424802343179,
4.15443361376849));
#35352=CARTESIAN_POINT('Ctrl Pts',(-6.30843407390273E-15,3.69113542328933,
4.27759390975198));
#35353=CARTESIAN_POINT('Ctrl Pts',(-8.95192615878647E-15,3.57253430986338,
4.3956575217037));
#35354=CARTESIAN_POINT('Ctrl Pts',(-1.17961196366423E-14,3.44872813349398,
4.50820230933582));
#35355=CARTESIAN_POINT('Ctrl Pts',(-1.37944585530683E-14,3.35923703106024,
4.58955331631885));
#35356=CARTESIAN_POINT('Ctrl Pts',(1.94969968696725E-15,3.26702518967802,
4.66802026523585));
#35357=CARTESIAN_POINT('Ctrl Pts',(2.41473507855972E-15,3.17225699350504,
4.74353062519992));
#35358=CARTESIAN_POINT('Ctrl Pts',(2.61939892934227E-15,3.13054914865896,
4.77676302282734));
#35359=CARTESIAN_POINT('Ctrl Pts',(-4.91819235567617E-15,3.08834600239139,
4.80942259857627));
#35360=CARTESIAN_POINT('Ctrl Pts',(-4.74620343027254E-15,3.0456608739011,
4.8415023979526));
#35361=CARTESIAN_POINT('Ctrl Pts',(-4.638233594795E-15,3.01886434447562,
4.86164119847529));
#35362=CARTESIAN_POINT('Ctrl Pts',(-1.61449114338701E-14,2.99187785892113,
4.8815515007876));
#35363=CARTESIAN_POINT('Ctrl Pts',(-1.5779044737485E-14,2.96470463632097,
4.90123148272646));
#35364=CARTESIAN_POINT('Ctrl Pts',(-1.55471922837076E-14,2.94748476252777,
4.91370283403529));
#35365=CARTESIAN_POINT('Ctrl Pts',(-1.43437538502047E-14,2.93018925838119,
4.92608207797112));
#35366=CARTESIAN_POINT('Ctrl Pts',(-1.45161660469739E-14,2.91283233270296,
4.93835944710776));
#35367=CARTESIAN_POINT('Ctrl Pts',(-1.58262398775716E-14,2.78094575775771,
5.03164901893566));
#35368=CARTESIAN_POINT('Ctrl Pts',(-8.3751524115744E-15,2.64533737784887,
5.1191898859788));
#35369=CARTESIAN_POINT('Ctrl Pts',(-8.17401701880272E-15,2.50645976707215,
5.20087831118996));
#35370=CARTESIAN_POINT('Ctrl Pts',(-7.96868972380821E-15,2.36468778073431,
5.28426922091417));
#35371=CARTESIAN_POINT('Ctrl Pts',(-3.28750966826451E-14,2.21950841305984,
5.36156169934779));
#35372=CARTESIAN_POINT('Ctrl Pts',(-2.99482660892636E-14,2.07135972951188,
5.43261292336788));
#35373=CARTESIAN_POINT('Ctrl Pts',(-2.7010140735854E-14,1.92263933408113,
5.50393833699321));
#35374=CARTESIAN_POINT('Ctrl Pts',(-9.29007357318986E-15,1.77092604516859,
5.56897467112021));
#35375=CARTESIAN_POINT('Ctrl Pts',(-1.16365250768524E-14,1.61662808464398,
5.62753811018193));
#35376=CARTESIAN_POINT('Ctrl Pts',(-1.39647681338263E-14,1.46352747517648,
5.68564709738033));
#35377=CARTESIAN_POINT('Ctrl Pts',(-2.80861324317553E-15,1.3078814874935,
5.73738362050802));
#35378=CARTESIAN_POINT('Ctrl Pts',(-2.63331023653279E-15,1.15006424595524,
5.78252360898802));
#35379=CARTESIAN_POINT('Ctrl Pts',(-2.54208608144777E-15,1.06793933097009,
5.80601355013904));
#35380=CARTESIAN_POINT('Ctrl Pts',(-8.84559606733975E-15,0.985226104351652,
5.82771641374748));
#35381=CARTESIAN_POINT('Ctrl Pts',(-8.93729534823251E-15,0.901975524283881,
5.84759529345977));
#35382=CARTESIAN_POINT('Ctrl Pts',(-1.68094704822153E-14,0.901975524284047,
5.84759529345974));
#35383=CARTESIAN_POINT('Ctrl Pts',(-0.0464195480276284,1.8765612251201,
5.69726812402404));
#35384=CARTESIAN_POINT('Ctrl Pts',(-0.0928390960552399,2.81234038373308,
5.29865417244734));
#35385=CARTESIAN_POINT('Ctrl Pts',(-0.13925864408285,3.59529440116169,4.69979479235976));
#35386=CARTESIAN_POINT('Ctrl Pts',(-0.18567819211046,4.3782484185903,4.10093541227217));
#35387=CARTESIAN_POINT('Ctrl Pts',(-0.232097740138068,5.00837729483454,
3.30183060367369));
#35388=CARTESIAN_POINT('Ctrl Pts',(-0.27851728816568,5.40837521702949,2.40072698448045));
#35389=CARTESIAN_POINT('Ctrl Pts',(-0.324936836193292,5.80837313922444,
1.49962336528722));
#35390=CARTESIAN_POINT('Ctrl Pts',(-0.371356384220907,5.9782401073701,0.496520935499224));
#35391=CARTESIAN_POINT('Ctrl Pts',(-0.417775932248519,5.8972621654928,-0.485971441301911));
#35392=CARTESIAN_POINT('Ctrl Pts',(-0.464195480276132,5.8162842236155,-1.46846381810305));
#35393=CARTESIAN_POINT('Ctrl Pts',(-0.510615028303743,5.48446137171524,
-2.43034614191732));
#35394=CARTESIAN_POINT('Ctrl Pts',(-0.557034576331353,4.94237295361224,
-3.25377865988359));
#35395=CARTESIAN_POINT('Ctrl Pts',(-0.603454124358963,4.40028453550923,
-4.07721117784986));
#35396=CARTESIAN_POINT('Ctrl Pts',(-0.649873672386574,3.64793055120348,
-4.76219388996812));
#35397=CARTESIAN_POINT('Ctrl Pts',(-0.696293220414184,2.77743042301163,
-5.22492199455547));
#35398=CARTESIAN_POINT('Ctrl Pts',(-0.742712768441798,1.90693029481972,
-5.68765009914285));
#35399=CARTESIAN_POINT('Ctrl Pts',(-0.789132316469411,0.918284022741709,
-5.92812359619928));
#35400=CARTESIAN_POINT('Ctrl Pts',(-0.835551864497027,-0.0674947272534869,
-5.91688120200961));
#35401=CARTESIAN_POINT('Ctrl Pts',(-0.881971412524643,-1.05327347724868,
-5.90563880781993));
#35402=CARTESIAN_POINT('Ctrl Pts',(-0.928390960552261,-2.03618470516106,
-5.64268052238414));
#35403=CARTESIAN_POINT('Ctrl Pts',(-0.974810508579875,-2.89590077580765,
-5.16020841554193));
#35404=CARTESIAN_POINT('Ctrl Pts',(-1.02123005660749,-3.75561684645419,
-4.67773630869973));
#35405=CARTESIAN_POINT('Ctrl Pts',(-1.06764960463509,-4.49213775983495,
-3.97575038045114));
#35406=CARTESIAN_POINT('Ctrl Pts',(-1.1140691526627,-5.01530574290011,-3.14017733058129));
#35407=CARTESIAN_POINT('Ctrl Pts',(-1.16048870069031,-5.53847372596528,
-2.30460428071143));
#35408=CARTESIAN_POINT('Ctrl Pts',(-1.20690824871793,-5.84828877871485,
-1.33544410922033));
#35409=CARTESIAN_POINT('Ctrl Pts',(-1.25332779674554,-5.90682374005196,
-0.351338921506704));
#35410=CARTESIAN_POINT('Ctrl Pts',(-1.25884346709541,-5.91377898982057,
-0.234405430430919));
#35411=CARTESIAN_POINT('Ctrl Pts',(-1.26435913744529,-5.91718649071705,
-0.117260935116202));
#35412=CARTESIAN_POINT('Ctrl Pts',(-1.26987480779516,-5.91708582682028,
-0.000110601437552926));
#35413=CARTESIAN_POINT('Origin',(0.5,8.93855739141052,-1.42379484493389));
#35414=CARTESIAN_POINT('',(11.,8.88202841720304,-1.45243629670899));
#35415=CARTESIAN_POINT('',(0.500000000000002,8.88202841720304,-1.45243629670899));
#35416=CARTESIAN_POINT('',(5.75,8.88202841720304,-1.45243629670899));
#35417=CARTESIAN_POINT('',(11.,8.71554861415804,-1.53678637235233));
#35418=CARTESIAN_POINT('',(11.,8.93855739141052,-1.42379484493389));
#35419=CARTESIAN_POINT('',(0.5,8.71554861415804,-1.53678637235233));
#35420=CARTESIAN_POINT('',(0.5,8.71554861415804,-1.53678637235233));
#35421=CARTESIAN_POINT('',(0.5,8.93855739141052,-1.42379484493389));
#35422=CARTESIAN_POINT('Origin',(0.5,8.81402938945926,-1.55415119011903));
#35423=CARTESIAN_POINT('',(0.5,8.84313903162825,-1.67298896209539));
#35424=CARTESIAN_POINT('Origin',(0.5,0.,0.));
#35425=CARTESIAN_POINT('',(0.5,8.71554861415804,-1.53678637235233));
#35426=CARTESIAN_POINT('Origin',(0.5,8.71554861415804,-1.53678637235233));
#35427=CARTESIAN_POINT('',(11.,8.84313903162825,-1.67298896209539));
#35428=CARTESIAN_POINT('',(5.75,8.84313903162825,-1.67298896209539));
#35429=CARTESIAN_POINT('',(11.,8.71554861415804,-1.53678637235233));
#35430=CARTESIAN_POINT('Origin',(11.,8.81402938945926,-1.55415119011903));
#35431=CARTESIAN_POINT('Origin',(11.,0.,0.));
#35432=CARTESIAN_POINT('Origin',(0.5,8.55552123961132,-2.95432840397942));
#35433=CARTESIAN_POINT('',(11.,8.49487753163548,-2.97271857438856));
#35434=CARTESIAN_POINT('',(0.5,8.49487753163548,-2.97271857438856));
#35435=CARTESIAN_POINT('',(5.75,8.49487753163548,-2.97271857438856));
#35436=CARTESIAN_POINT('',(11.,8.31627969395529,-3.02687826843217));
#35437=CARTESIAN_POINT('',(11.,8.55552123961132,-2.95432840397942));
#35438=CARTESIAN_POINT('',(0.5,8.31627969395529,-3.02687826843217));
#35439=CARTESIAN_POINT('',(0.5,8.31627969395529,-3.02687826843217));
#35440=CARTESIAN_POINT('',(0.5,8.55552123961132,-2.95432840397942));
#35441=CARTESIAN_POINT('Origin',(0.5,8.41024895603388,-3.06108028276474));
#35442=CARTESIAN_POINT('',(0.5,8.41828039478761,-3.18316747827294));
#35443=CARTESIAN_POINT('Origin',(0.5,0.,0.));
#35444=CARTESIAN_POINT('',(0.5,8.31627969395529,-3.02687826843217));
#35445=CARTESIAN_POINT('Origin',(0.5,8.31627969395529,-3.02687826843217));
#35446=CARTESIAN_POINT('',(11.,8.41828039478761,-3.18316747827294));
#35447=CARTESIAN_POINT('',(5.75,8.41828039478761,-3.18316747827294));
#35448=CARTESIAN_POINT('',(11.,8.31627969395529,-3.02687826843217));
#35449=CARTESIAN_POINT('Origin',(11.,8.41024895603388,-3.06108028276474));
#35450=CARTESIAN_POINT('Origin',(11.,0.,0.));
#35451=CARTESIAN_POINT('Origin',(0.5,7.91252990424917,-4.39509618943234));
#35452=CARTESIAN_POINT('',(11.,7.84961409088462,-4.4026763024535));
#35453=CARTESIAN_POINT('',(0.5,7.84961409088462,-4.4026763024535));
#35454=CARTESIAN_POINT('',(5.75,7.84961409088462,-4.4026763024535));
#35455=CARTESIAN_POINT('',(11.,7.66432482349228,-4.425));
#35456=CARTESIAN_POINT('',(11.,7.91252990424917,-4.39509618943234));
#35457=CARTESIAN_POINT('',(0.5,7.66432482349228,-4.425));
#35458=CARTESIAN_POINT('',(0.5,7.66432482349228,-4.425));
#35459=CARTESIAN_POINT('',(0.5,7.91252990424917,-4.39509618943234));
#35460=CARTESIAN_POINT('Origin',(0.5,7.75092736387072,-4.475));
#35461=CARTESIAN_POINT('',(0.5,7.73763656800678,-4.59662706138363));
#35462=CARTESIAN_POINT('Origin',(0.5,0.,0.));
#35463=CARTESIAN_POINT('',(0.5,7.66432482349228,-4.425));
#35464=CARTESIAN_POINT('Origin',(0.5,7.66432482349228,-4.425));
#35465=CARTESIAN_POINT('',(11.,7.73763656800678,-4.59662706138363));
#35466=CARTESIAN_POINT('',(5.75,7.73763656800678,-4.59662706138363));
#35467=CARTESIAN_POINT('',(11.,7.66432482349228,-4.425));
#35468=CARTESIAN_POINT('Origin',(11.,7.75092736387072,-4.475));
#35469=CARTESIAN_POINT('Origin',(11.,0.,0.));
#35470=CARTESIAN_POINT('Origin',(0.5,7.02912035167973,-5.70232120119534));
#35471=CARTESIAN_POINT('',(11.,6.96584409807862,-5.6988609389301));
#35472=CARTESIAN_POINT('',(0.5,6.96584409807862,-5.6988609389301));
#35473=CARTESIAN_POINT('',(5.75,6.96584409807862,-5.6988609389301));
#35474=CARTESIAN_POINT('',(11.,6.77949332160295,-5.68867034572588));
#35475=CARTESIAN_POINT('',(11.,7.02912035167973,-5.70232120119534));
#35476=CARTESIAN_POINT('',(0.5,6.77949332160295,-5.68867034572588));
#35477=CARTESIAN_POINT('',(0.5,6.77949332160295,-5.68867034572588));
#35478=CARTESIAN_POINT('',(0.5,7.02912035167973,-5.70232120119534));
#35479=CARTESIAN_POINT('Origin',(0.5,6.85609776591485,-5.75294910669453));
#35480=CARTESIAN_POINT('',(0.5,6.82188856954008,-5.8704204572397));
#35481=CARTESIAN_POINT('Origin',(0.5,0.,0.));
#35482=CARTESIAN_POINT('',(0.5,6.77949332160295,-5.68867034572588));
#35483=CARTESIAN_POINT('Origin',(0.5,6.77949332160295,-5.68867034572588));
#35484=CARTESIAN_POINT('',(11.,6.82188856954008,-5.8704204572397));
#35485=CARTESIAN_POINT('',(5.75,6.82188856954008,-5.8704204572397));
#35486=CARTESIAN_POINT('',(11.,6.77949332160295,-5.68867034572588));
#35487=CARTESIAN_POINT('Origin',(11.,6.85609776591485,-5.75294910669453));
#35488=CARTESIAN_POINT('Origin',(11.,0.,0.));
#35489=CARTESIAN_POINT('Origin',(0.5,5.93213453413103,-6.83628406877377));
#35490=CARTESIAN_POINT('',(11.,5.87042045723969,-6.82188856954009));
#35491=CARTESIAN_POINT('',(0.5,5.87042045723969,-6.82188856954009));
#35492=CARTESIAN_POINT('',(5.75,5.87042045723969,-6.82188856954009));
#35493=CARTESIAN_POINT('',(11.,5.68867034572587,-6.77949332160296));
#35494=CARTESIAN_POINT('',(11.,5.93213453413103,-6.83628406877377));
#35495=CARTESIAN_POINT('',(0.5,5.68867034572587,-6.77949332160296));
#35496=CARTESIAN_POINT('',(0.5,5.68867034572587,-6.77949332160296));
#35497=CARTESIAN_POINT('',(0.5,5.93213453413103,-6.83628406877377));
#35498=CARTESIAN_POINT('Origin',(0.5,5.75294910669453,-6.85609776591486));
#35499=CARTESIAN_POINT('',(0.5,5.6988609389301,-6.96584409807862));
#35500=CARTESIAN_POINT('Origin',(0.5,0.,0.));
#35501=CARTESIAN_POINT('',(0.5,5.68867034572587,-6.77949332160296));
#35502=CARTESIAN_POINT('Origin',(0.5,5.68867034572587,-6.77949332160296));
#35503=CARTESIAN_POINT('',(11.,5.6988609389301,-6.96584409807862));
#35504=CARTESIAN_POINT('',(5.75,5.6988609389301,-6.96584409807862));
#35505=CARTESIAN_POINT('',(11.,5.68867034572587,-6.77949332160296));
#35506=CARTESIAN_POINT('Origin',(11.,5.75294910669453,-6.85609776591486));
#35507=CARTESIAN_POINT('Origin',(11.,0.,0.));
#35508=CARTESIAN_POINT('Origin',(0.5,4.65490381056767,-7.76252990424917));
#35509=CARTESIAN_POINT('',(11.,4.59662706138363,-7.73763656800678));
#35510=CARTESIAN_POINT('',(0.5,4.59662706138363,-7.73763656800678));
#35511=CARTESIAN_POINT('',(5.75,4.59662706138363,-7.73763656800678));
#35512=CARTESIAN_POINT('',(11.,4.425,-7.66432482349228));
#35513=CARTESIAN_POINT('',(11.,4.65490381056767,-7.76252990424917));
#35514=CARTESIAN_POINT('',(0.5,4.425,-7.66432482349228));
#35515=CARTESIAN_POINT('',(0.5,4.425,-7.66432482349228));
#35516=CARTESIAN_POINT('',(0.5,4.65490381056767,-7.76252990424917));
#35517=CARTESIAN_POINT('Origin',(0.5,4.475,-7.75092736387073));
#35518=CARTESIAN_POINT('',(0.5,4.4026763024535,-7.84961409088462));
#35519=CARTESIAN_POINT('Origin',(0.5,0.,0.));
#35520=CARTESIAN_POINT('',(0.5,4.425,-7.66432482349228));
#35521=CARTESIAN_POINT('Origin',(0.5,4.425,-7.66432482349228));
#35522=CARTESIAN_POINT('',(11.,4.4026763024535,-7.84961409088462));
#35523=CARTESIAN_POINT('',(5.75,4.4026763024535,-7.84961409088462));
#35524=CARTESIAN_POINT('',(11.,4.425,-7.66432482349228));
#35525=CARTESIAN_POINT('Origin',(11.,4.475,-7.75092736387073));
#35526=CARTESIAN_POINT('Origin',(11.,0.,0.));
#35527=CARTESIAN_POINT('Origin',(0.5,3.23623619021518,-8.45291519661362));
#35528=CARTESIAN_POINT('',(11.,3.18316747827293,-8.41828039478762));
#35529=CARTESIAN_POINT('',(0.5,3.18316747827293,-8.41828039478762));
#35530=CARTESIAN_POINT('',(5.75,3.18316747827293,-8.41828039478762));
#35531=CARTESIAN_POINT('',(11.,3.02687826843216,-8.31627969395529));
#35532=CARTESIAN_POINT('',(11.,3.23623619021518,-8.45291519661362));
#35533=CARTESIAN_POINT('',(0.5,3.02687826843216,-8.31627969395529));
#35534=CARTESIAN_POINT('',(0.5,3.02687826843216,-8.31627969395529));
#35535=CARTESIAN_POINT('',(0.5,3.23623619021518,-8.45291519661362));
#35536=CARTESIAN_POINT('Origin',(0.5,3.06108028276473,-8.41024895603388));
#35537=CARTESIAN_POINT('',(0.500000000000002,2.97271857438855,-8.49487753163548));
#35538=CARTESIAN_POINT('Origin',(0.5,0.,0.));
#35539=CARTESIAN_POINT('',(0.5,3.02687826843216,-8.31627969395529));
#35540=CARTESIAN_POINT('Origin',(0.5,3.02687826843216,-8.31627969395529));
#35541=CARTESIAN_POINT('',(11.,2.97271857438855,-8.49487753163548));
#35542=CARTESIAN_POINT('',(5.75,2.97271857438855,-8.49487753163548));
#35543=CARTESIAN_POINT('',(11.,3.02687826843216,-8.31627969395529));
#35544=CARTESIAN_POINT('Origin',(11.,3.06108028276473,-8.41024895603388));
#35545=CARTESIAN_POINT('Origin',(11.,0.,0.));
#35546=CARTESIAN_POINT('Origin',(0.5,1.71923717083755,-8.88646293811044));
#35547=CARTESIAN_POINT('',(11.,1.67298896209539,-8.84313903162825));
#35548=CARTESIAN_POINT('',(0.5,1.67298896209539,-8.84313903162825));
#35549=CARTESIAN_POINT('',(5.75,1.67298896209539,-8.84313903162825));
#35550=CARTESIAN_POINT('',(11.,1.53678637235233,-8.71554861415804));
#35551=CARTESIAN_POINT('',(11.,1.71923717083755,-8.88646293811044));
#35552=CARTESIAN_POINT('',(0.5,1.53678637235233,-8.71554861415804));
#35553=CARTESIAN_POINT('',(0.5,1.53678637235233,-8.71554861415804));
#35554=CARTESIAN_POINT('',(0.5,1.71923717083755,-8.88646293811044));
#35555=CARTESIAN_POINT('Origin',(0.5,1.55415119011902,-8.81402938945926));
#35556=CARTESIAN_POINT('',(0.5,1.45243629670899,-8.88202841720304));
#35557=CARTESIAN_POINT('Origin',(0.5,0.,0.));
#35558=CARTESIAN_POINT('',(0.5,1.53678637235233,-8.71554861415804));
#35559=CARTESIAN_POINT('Origin',(0.5,1.53678637235233,-8.71554861415804));
#35560=CARTESIAN_POINT('',(11.,1.45243629670899,-8.88202841720304));
#35561=CARTESIAN_POINT('',(5.75,1.45243629670899,-8.88202841720304));
#35562=CARTESIAN_POINT('',(11.,1.53678637235233,-8.71554861415804));
#35563=CARTESIAN_POINT('Origin',(11.,1.55415119011902,-8.81402938945926));
#35564=CARTESIAN_POINT('Origin',(11.,0.,0.));
#35565=CARTESIAN_POINT('Origin',(0.5,0.149999999999998,-9.05));
#35566=CARTESIAN_POINT('',(11.,0.111977522877841,-8.99930336383712));
#35567=CARTESIAN_POINT('',(0.5,0.111977522877841,-8.99930336383712));
#35568=CARTESIAN_POINT('',(5.75,0.11197752287784,-8.99930336383712));
#35569=CARTESIAN_POINT('',(11.,-1.62571862586811E-15,-8.85));
#35570=CARTESIAN_POINT('',(11.,0.149999999999998,-9.05));
#35571=CARTESIAN_POINT('',(0.5,-1.62571862586811E-15,-8.85));
#35572=CARTESIAN_POINT('',(0.5,-1.62571862586811E-15,-8.85));
#35573=CARTESIAN_POINT('',(0.5,0.149999999999998,-9.05));
#35574=CARTESIAN_POINT('Origin',(0.5,-1.64408832785532E-15,-8.95));
#35575=CARTESIAN_POINT('',(0.5,-0.111977522877842,-8.99930336383712));
#35576=CARTESIAN_POINT('Origin',(0.5,0.,0.));
#35577=CARTESIAN_POINT('',(0.5,-1.62571862586811E-15,-8.85));
#35578=CARTESIAN_POINT('Origin',(0.5,-1.62571862586811E-15,-8.85));
#35579=CARTESIAN_POINT('',(11.,-0.111977522877842,-8.99930336383712));
#35580=CARTESIAN_POINT('',(5.75,-0.111977522877842,-8.99930336383712));
#35581=CARTESIAN_POINT('',(11.,-1.62571862586811E-15,-8.85));
#35582=CARTESIAN_POINT('Origin',(11.,-1.64408832785532E-15,-8.95));
#35583=CARTESIAN_POINT('Origin',(11.,0.,0.));
#35584=CARTESIAN_POINT('Origin',(0.5,-1.42379484493389,-8.93855739141052));
#35585=CARTESIAN_POINT('',(11.,-1.45243629670899,-8.88202841720304));
#35586=CARTESIAN_POINT('',(0.5,-1.45243629670899,-8.88202841720304));
#35587=CARTESIAN_POINT('',(5.75,-1.45243629670899,-8.88202841720304));
#35588=CARTESIAN_POINT('',(11.,-1.53678637235233,-8.71554861415804));
#35589=CARTESIAN_POINT('',(11.,-1.42379484493389,-8.93855739141052));
#35590=CARTESIAN_POINT('',(0.5,-1.53678637235233,-8.71554861415804));
#35591=CARTESIAN_POINT('',(0.5,-1.53678637235233,-8.71554861415804));
#35592=CARTESIAN_POINT('',(0.5,-1.42379484493389,-8.93855739141052));
#35593=CARTESIAN_POINT('Origin',(0.5,-1.55415119011903,-8.81402938945926));
#35594=CARTESIAN_POINT('',(0.5,-1.67298896209539,-8.84313903162825));
#35595=CARTESIAN_POINT('Origin',(0.5,0.,0.));
#35596=CARTESIAN_POINT('',(0.5,-1.53678637235233,-8.71554861415804));
#35597=CARTESIAN_POINT('Origin',(0.5,-1.53678637235233,-8.71554861415804));
#35598=CARTESIAN_POINT('',(11.,-1.67298896209539,-8.84313903162825));
#35599=CARTESIAN_POINT('',(5.75,-1.67298896209539,-8.84313903162825));
#35600=CARTESIAN_POINT('',(11.,-1.53678637235233,-8.71554861415804));
#35601=CARTESIAN_POINT('Origin',(11.,-1.55415119011903,-8.81402938945926));
#35602=CARTESIAN_POINT('Origin',(11.,0.,0.));
#35603=CARTESIAN_POINT('Origin',(0.5,-2.95432840397942,-8.55552123961132));
#35604=CARTESIAN_POINT('',(11.,-2.97271857438856,-8.49487753163548));
#35605=CARTESIAN_POINT('',(0.5,-2.97271857438856,-8.49487753163548));
#35606=CARTESIAN_POINT('',(5.75,-2.97271857438856,-8.49487753163548));
#35607=CARTESIAN_POINT('',(11.,-3.02687826843217,-8.31627969395529));
#35608=CARTESIAN_POINT('',(11.,-2.95432840397942,-8.55552123961132));
#35609=CARTESIAN_POINT('',(0.5,-3.02687826843217,-8.31627969395529));
#35610=CARTESIAN_POINT('',(0.5,-3.02687826843217,-8.31627969395529));
#35611=CARTESIAN_POINT('',(0.5,-2.95432840397942,-8.55552123961132));
#35612=CARTESIAN_POINT('Origin',(0.5,-3.06108028276474,-8.41024895603388));
#35613=CARTESIAN_POINT('',(0.5,-3.18316747827294,-8.41828039478761));
#35614=CARTESIAN_POINT('Origin',(0.5,0.,0.));
#35615=CARTESIAN_POINT('',(0.5,-3.02687826843217,-8.31627969395529));
#35616=CARTESIAN_POINT('Origin',(0.5,-3.02687826843217,-8.31627969395529));
#35617=CARTESIAN_POINT('',(11.,-3.18316747827294,-8.41828039478761));
#35618=CARTESIAN_POINT('',(5.75,-3.18316747827294,-8.41828039478761));
#35619=CARTESIAN_POINT('',(11.,-3.02687826843217,-8.31627969395529));
#35620=CARTESIAN_POINT('Origin',(11.,-3.06108028276474,-8.41024895603388));
#35621=CARTESIAN_POINT('Origin',(11.,0.,0.));
#35622=CARTESIAN_POINT('Origin',(0.5,-4.39509618943234,-7.91252990424917));
#35623=CARTESIAN_POINT('',(11.,-4.4026763024535,-7.84961409088462));
#35624=CARTESIAN_POINT('',(0.5,-4.4026763024535,-7.84961409088462));
#35625=CARTESIAN_POINT('',(5.75,-4.4026763024535,-7.84961409088462));
#35626=CARTESIAN_POINT('',(11.,-4.425,-7.66432482349228));
#35627=CARTESIAN_POINT('',(11.,-4.39509618943234,-7.91252990424917));
#35628=CARTESIAN_POINT('',(0.5,-4.425,-7.66432482349228));
#35629=CARTESIAN_POINT('',(0.5,-4.425,-7.66432482349228));
#35630=CARTESIAN_POINT('',(0.5,-4.39509618943234,-7.91252990424917));
#35631=CARTESIAN_POINT('Origin',(0.5,-4.475,-7.75092736387072));
#35632=CARTESIAN_POINT('',(0.5,-4.59662706138363,-7.73763656800678));
#35633=CARTESIAN_POINT('Origin',(0.5,0.,0.));
#35634=CARTESIAN_POINT('',(0.5,-4.425,-7.66432482349228));
#35635=CARTESIAN_POINT('Origin',(0.5,-4.425,-7.66432482349228));
#35636=CARTESIAN_POINT('',(11.,-4.59662706138363,-7.73763656800678));
#35637=CARTESIAN_POINT('',(5.75,-4.59662706138363,-7.73763656800678));
#35638=CARTESIAN_POINT('',(11.,-4.425,-7.66432482349228));
#35639=CARTESIAN_POINT('Origin',(11.,-4.475,-7.75092736387072));
#35640=CARTESIAN_POINT('Origin',(11.,0.,0.));
#35641=CARTESIAN_POINT('Origin',(0.5,-5.70232120119534,-7.02912035167973));
#35642=CARTESIAN_POINT('',(11.,-5.6988609389301,-6.96584409807862));
#35643=CARTESIAN_POINT('',(0.5,-5.6988609389301,-6.96584409807862));
#35644=CARTESIAN_POINT('',(5.75,-5.6988609389301,-6.96584409807862));
#35645=CARTESIAN_POINT('',(11.,-5.68867034572587,-6.77949332160295));
#35646=CARTESIAN_POINT('',(11.,-5.70232120119534,-7.02912035167973));
#35647=CARTESIAN_POINT('',(0.5,-5.68867034572587,-6.77949332160295));
#35648=CARTESIAN_POINT('',(0.5,-5.68867034572587,-6.77949332160295));
#35649=CARTESIAN_POINT('',(0.5,-5.70232120119534,-7.02912035167973));
#35650=CARTESIAN_POINT('Origin',(0.5,-5.75294910669453,-6.85609776591485));
#35651=CARTESIAN_POINT('',(0.5,-5.8704204572397,-6.82188856954009));
#35652=CARTESIAN_POINT('Origin',(0.5,0.,0.));
#35653=CARTESIAN_POINT('',(0.5,-5.68867034572587,-6.77949332160295));
#35654=CARTESIAN_POINT('Origin',(0.5,-5.68867034572587,-6.77949332160295));
#35655=CARTESIAN_POINT('',(11.,-5.8704204572397,-6.82188856954009));
#35656=CARTESIAN_POINT('',(5.75,-5.8704204572397,-6.82188856954009));
#35657=CARTESIAN_POINT('',(11.,-5.68867034572587,-6.77949332160295));
#35658=CARTESIAN_POINT('Origin',(11.,-5.75294910669453,-6.85609776591485));
#35659=CARTESIAN_POINT('Origin',(11.,0.,0.));
#35660=CARTESIAN_POINT('Origin',(0.5,-6.83628406877377,-5.93213453413103));
#35661=CARTESIAN_POINT('',(11.,-6.82188856954009,-5.8704204572397));
#35662=CARTESIAN_POINT('',(0.500000000000002,-6.82188856954009,-5.8704204572397));
#35663=CARTESIAN_POINT('',(5.75,-6.82188856954009,-5.8704204572397));
#35664=CARTESIAN_POINT('',(11.,-6.77949332160296,-5.68867034572587));
#35665=CARTESIAN_POINT('',(11.,-6.83628406877377,-5.93213453413103));
#35666=CARTESIAN_POINT('',(0.5,-6.77949332160296,-5.68867034572587));
#35667=CARTESIAN_POINT('',(0.5,-6.77949332160296,-5.68867034572587));
#35668=CARTESIAN_POINT('',(0.5,-6.83628406877377,-5.93213453413103));
#35669=CARTESIAN_POINT('Origin',(0.5,-6.85609776591486,-5.75294910669453));
#35670=CARTESIAN_POINT('',(0.5,-6.96584409807862,-5.6988609389301));
#35671=CARTESIAN_POINT('Origin',(0.5,0.,0.));
#35672=CARTESIAN_POINT('',(0.5,-6.77949332160296,-5.68867034572587));
#35673=CARTESIAN_POINT('Origin',(0.5,-6.77949332160296,-5.68867034572587));
#35674=CARTESIAN_POINT('',(11.,-6.96584409807862,-5.6988609389301));
#35675=CARTESIAN_POINT('',(5.75,-6.96584409807862,-5.6988609389301));
#35676=CARTESIAN_POINT('',(11.,-6.77949332160296,-5.68867034572587));
#35677=CARTESIAN_POINT('Origin',(11.,-6.85609776591486,-5.75294910669453));
#35678=CARTESIAN_POINT('Origin',(11.,0.,0.));
#35679=CARTESIAN_POINT('Origin',(0.5,-7.76252990424917,-4.65490381056766));
#35680=CARTESIAN_POINT('',(11.,-7.73763656800678,-4.59662706138362));
#35681=CARTESIAN_POINT('',(0.5,-7.73763656800678,-4.59662706138362));
#35682=CARTESIAN_POINT('',(5.75,-7.73763656800678,-4.59662706138362));
#35683=CARTESIAN_POINT('',(11.,-7.66432482349228,-4.425));
#35684=CARTESIAN_POINT('',(11.,-7.76252990424917,-4.65490381056766));
#35685=CARTESIAN_POINT('',(0.5,-7.66432482349228,-4.425));
#35686=CARTESIAN_POINT('',(0.5,-7.66432482349228,-4.425));
#35687=CARTESIAN_POINT('',(0.5,-7.76252990424917,-4.65490381056766));
#35688=CARTESIAN_POINT('Origin',(0.5,-7.75092736387073,-4.475));
#35689=CARTESIAN_POINT('',(0.5,-7.84961409088462,-4.40267630245349));
#35690=CARTESIAN_POINT('Origin',(0.5,0.,0.));
#35691=CARTESIAN_POINT('',(0.5,-7.66432482349228,-4.425));
#35692=CARTESIAN_POINT('Origin',(0.5,-7.66432482349228,-4.425));
#35693=CARTESIAN_POINT('',(11.,-7.84961409088462,-4.40267630245349));
#35694=CARTESIAN_POINT('',(5.75,-7.84961409088462,-4.40267630245349));
#35695=CARTESIAN_POINT('',(11.,-7.66432482349228,-4.425));
#35696=CARTESIAN_POINT('Origin',(11.,-7.75092736387073,-4.475));
#35697=CARTESIAN_POINT('Origin',(11.,0.,0.));
#35698=CARTESIAN_POINT('Origin',(0.5,-8.45291519661362,-3.23623619021519));
#35699=CARTESIAN_POINT('',(11.,-8.41828039478761,-3.18316747827294));
#35700=CARTESIAN_POINT('',(0.5,-8.41828039478761,-3.18316747827294));
#35701=CARTESIAN_POINT('',(5.75,-8.41828039478761,-3.18316747827294));
#35702=CARTESIAN_POINT('',(11.,-8.31627969395529,-3.02687826843217));
#35703=CARTESIAN_POINT('',(11.,-8.45291519661362,-3.23623619021519));
#35704=CARTESIAN_POINT('',(0.5,-8.31627969395529,-3.02687826843217));
#35705=CARTESIAN_POINT('',(0.5,-8.31627969395529,-3.02687826843217));
#35706=CARTESIAN_POINT('',(0.5,-8.45291519661362,-3.23623619021519));
#35707=CARTESIAN_POINT('Origin',(0.5,-8.41024895603388,-3.06108028276473));
#35708=CARTESIAN_POINT('',(0.5,-8.49487753163548,-2.97271857438855));
#35709=CARTESIAN_POINT('Origin',(0.5,0.,0.));
#35710=CARTESIAN_POINT('',(0.5,-8.31627969395529,-3.02687826843217));
#35711=CARTESIAN_POINT('Origin',(0.5,-8.31627969395529,-3.02687826843217));
#35712=CARTESIAN_POINT('',(11.,-8.49487753163548,-2.97271857438855));
#35713=CARTESIAN_POINT('',(5.75,-8.49487753163548,-2.97271857438855));
#35714=CARTESIAN_POINT('',(11.,-8.31627969395529,-3.02687826843217));
#35715=CARTESIAN_POINT('Origin',(11.,-8.41024895603388,-3.06108028276473));
#35716=CARTESIAN_POINT('Origin',(11.,0.,0.));
#35717=CARTESIAN_POINT('Origin',(0.5,-8.88646293811044,-1.71923717083755));
#35718=CARTESIAN_POINT('',(11.,-8.84313903162825,-1.67298896209539));
#35719=CARTESIAN_POINT('',(0.5,-8.84313903162825,-1.67298896209539));
#35720=CARTESIAN_POINT('',(5.75,-8.84313903162825,-1.67298896209539));
#35721=CARTESIAN_POINT('',(11.,-8.71554861415804,-1.53678637235233));
#35722=CARTESIAN_POINT('',(11.,-8.88646293811044,-1.71923717083755));
#35723=CARTESIAN_POINT('',(0.5,-8.71554861415804,-1.53678637235233));
#35724=CARTESIAN_POINT('',(0.5,-8.71554861415804,-1.53678637235233));
#35725=CARTESIAN_POINT('',(0.5,-8.88646293811044,-1.71923717083755));
#35726=CARTESIAN_POINT('Origin',(0.5,-8.81402938945926,-1.55415119011902));
#35727=CARTESIAN_POINT('',(0.5,-8.88202841720304,-1.45243629670899));
#35728=CARTESIAN_POINT('Origin',(0.5,0.,0.));
#35729=CARTESIAN_POINT('',(0.5,-8.71554861415804,-1.53678637235233));
#35730=CARTESIAN_POINT('Origin',(0.5,-8.71554861415804,-1.53678637235233));
#35731=CARTESIAN_POINT('',(11.,-8.88202841720304,-1.45243629670899));
#35732=CARTESIAN_POINT('',(5.75,-8.88202841720304,-1.45243629670899));
#35733=CARTESIAN_POINT('',(11.,-8.71554861415804,-1.53678637235233));
#35734=CARTESIAN_POINT('Origin',(11.,-8.81402938945926,-1.55415119011902));
#35735=CARTESIAN_POINT('Origin',(11.,0.,0.));
#35736=CARTESIAN_POINT('Origin',(0.5,-9.05,-0.149999999999999));
#35737=CARTESIAN_POINT('',(11.,-8.99930336383712,-0.111977522877841));
#35738=CARTESIAN_POINT('',(0.5,-8.99930336383712,-0.111977522877841));
#35739=CARTESIAN_POINT('',(5.75,-8.99930336383712,-0.11197752287784));
#35740=CARTESIAN_POINT('',(11.,-8.85,1.08381241724541E-15));
#35741=CARTESIAN_POINT('',(11.,-9.05,-0.149999999999999));
#35742=CARTESIAN_POINT('',(0.5,-8.85,1.08381241724541E-15));
#35743=CARTESIAN_POINT('',(0.5,-8.85,1.08381241724541E-15));
#35744=CARTESIAN_POINT('',(0.5,-9.05,-0.149999999999999));
#35745=CARTESIAN_POINT('Origin',(0.5,-8.95,1.09605888523688E-15));
#35746=CARTESIAN_POINT('',(0.5,-9.,-1.10218211923262E-15));
#35747=CARTESIAN_POINT('Origin',(0.5,0.,0.));
#35748=CARTESIAN_POINT('',(0.5,-8.99930336383712,0.111977522877842));
#35749=CARTESIAN_POINT('',(0.5,-8.85,1.08381241724541E-15));
#35750=CARTESIAN_POINT('Origin',(0.5,0.,0.));
#35751=CARTESIAN_POINT('Origin',(0.5,-8.85,1.08381241724541E-15));
#35752=CARTESIAN_POINT('',(11.,-8.99930336383712,0.111977522877842));
#35753=CARTESIAN_POINT('',(5.75,-8.99930336383712,0.111977522877842));
#35754=CARTESIAN_POINT('',(11.,-8.85,1.08381241724541E-15));
#35755=CARTESIAN_POINT('Origin',(11.,-8.95,1.09605888523688E-15));
#35756=CARTESIAN_POINT('',(11.,-9.,-1.10218211923262E-15));
#35757=CARTESIAN_POINT('Origin',(11.,0.,0.));
#35758=CARTESIAN_POINT('Origin',(11.,0.,0.));
#35759=CARTESIAN_POINT('Origin',(0.5,-8.93855739141052,1.42379484493389));
#35760=CARTESIAN_POINT('',(11.,-8.88202841720304,1.45243629670899));
#35761=CARTESIAN_POINT('',(0.5,-8.88202841720304,1.45243629670899));
#35762=CARTESIAN_POINT('',(5.75,-8.88202841720304,1.45243629670899));
#35763=CARTESIAN_POINT('',(11.,-8.71554861415804,1.53678637235234));
#35764=CARTESIAN_POINT('',(11.,-8.93855739141052,1.42379484493389));
#35765=CARTESIAN_POINT('',(0.5,-8.71554861415804,1.53678637235234));
#35766=CARTESIAN_POINT('',(0.5,-8.71554861415804,1.53678637235234));
#35767=CARTESIAN_POINT('',(0.5,-8.93855739141052,1.42379484493389));
#35768=CARTESIAN_POINT('Origin',(0.5,-8.81402938945926,1.55415119011903));
#35769=CARTESIAN_POINT('',(0.5,-8.84313903162825,1.6729889620954));
#35770=CARTESIAN_POINT('Origin',(0.5,0.,0.));
#35771=CARTESIAN_POINT('',(0.5,-8.71554861415804,1.53678637235234));
#35772=CARTESIAN_POINT('Origin',(0.5,-8.71554861415804,1.53678637235234));
#35773=CARTESIAN_POINT('',(11.,-8.84313903162825,1.6729889620954));
#35774=CARTESIAN_POINT('',(5.75,-8.84313903162825,1.6729889620954));
#35775=CARTESIAN_POINT('',(11.,-8.71554861415804,1.53678637235234));
#35776=CARTESIAN_POINT('Origin',(11.,-8.81402938945926,1.55415119011903));
#35777=CARTESIAN_POINT('Origin',(11.,0.,0.));
#35778=CARTESIAN_POINT('Origin',(0.5,-8.55552123961132,2.95432840397942));
#35779=CARTESIAN_POINT('',(11.,-8.49487753163548,2.97271857438855));
#35780=CARTESIAN_POINT('',(0.5,-8.49487753163548,2.97271857438855));
#35781=CARTESIAN_POINT('',(5.75,-8.49487753163548,2.97271857438855));
#35782=CARTESIAN_POINT('',(11.,-8.31627969395529,3.02687826843217));
#35783=CARTESIAN_POINT('',(11.,-8.55552123961132,2.95432840397942));
#35784=CARTESIAN_POINT('',(0.5,-8.31627969395529,3.02687826843217));
#35785=CARTESIAN_POINT('',(0.5,-8.31627969395529,3.02687826843217));
#35786=CARTESIAN_POINT('',(0.5,-8.55552123961132,2.95432840397942));
#35787=CARTESIAN_POINT('Origin',(0.5,-8.41024895603388,3.06108028276474));
#35788=CARTESIAN_POINT('',(0.5,-8.41828039478761,3.18316747827294));
#35789=CARTESIAN_POINT('Origin',(0.5,0.,0.));
#35790=CARTESIAN_POINT('',(0.5,-8.31627969395529,3.02687826843217));
#35791=CARTESIAN_POINT('Origin',(0.5,-8.31627969395529,3.02687826843217));
#35792=CARTESIAN_POINT('',(11.,-8.41828039478761,3.18316747827294));
#35793=CARTESIAN_POINT('',(5.75,-8.41828039478761,3.18316747827294));
#35794=CARTESIAN_POINT('',(11.,-8.31627969395529,3.02687826843217));
#35795=CARTESIAN_POINT('Origin',(11.,-8.41024895603388,3.06108028276474));
#35796=CARTESIAN_POINT('Origin',(11.,0.,0.));
#35797=CARTESIAN_POINT('Origin',(0.5,-7.91252990424917,4.39509618943233));
#35798=CARTESIAN_POINT('',(11.,-7.84961409088462,4.4026763024535));
#35799=CARTESIAN_POINT('',(0.5,-7.84961409088462,4.4026763024535));
#35800=CARTESIAN_POINT('',(5.75,-7.84961409088462,4.4026763024535));
#35801=CARTESIAN_POINT('',(11.,-7.66432482349228,4.425));
#35802=CARTESIAN_POINT('',(11.,-7.91252990424917,4.39509618943233));
#35803=CARTESIAN_POINT('',(0.5,-7.66432482349228,4.425));
#35804=CARTESIAN_POINT('',(0.5,-7.66432482349228,4.425));
#35805=CARTESIAN_POINT('',(0.5,-7.91252990424917,4.39509618943233));
#35806=CARTESIAN_POINT('Origin',(0.5,-7.75092736387073,4.475));
#35807=CARTESIAN_POINT('',(0.5,-7.73763656800678,4.59662706138363));
#35808=CARTESIAN_POINT('Origin',(0.5,0.,0.));
#35809=CARTESIAN_POINT('',(0.5,-7.66432482349228,4.425));
#35810=CARTESIAN_POINT('Origin',(0.5,-7.66432482349228,4.425));
#35811=CARTESIAN_POINT('',(11.,-7.73763656800678,4.59662706138363));
#35812=CARTESIAN_POINT('',(5.75,-7.73763656800678,4.59662706138363));
#35813=CARTESIAN_POINT('',(11.,-7.66432482349228,4.425));
#35814=CARTESIAN_POINT('Origin',(11.,-7.75092736387073,4.475));
#35815=CARTESIAN_POINT('Origin',(11.,0.,0.));
#35816=CARTESIAN_POINT('Origin',(0.5,-7.02912035167973,5.70232120119534));
#35817=CARTESIAN_POINT('',(11.,-6.96584409807862,5.6988609389301));
#35818=CARTESIAN_POINT('',(0.5,-6.96584409807862,5.6988609389301));
#35819=CARTESIAN_POINT('',(5.75,-6.96584409807862,5.6988609389301));
#35820=CARTESIAN_POINT('',(11.,-6.77949332160295,5.68867034572587));
#35821=CARTESIAN_POINT('',(11.,-7.02912035167973,5.70232120119534));
#35822=CARTESIAN_POINT('',(0.5,-6.77949332160295,5.68867034572587));
#35823=CARTESIAN_POINT('',(0.5,-6.77949332160295,5.68867034572587));
#35824=CARTESIAN_POINT('',(0.5,-7.02912035167973,5.70232120119534));
#35825=CARTESIAN_POINT('Origin',(0.5,-6.85609776591485,5.75294910669453));
#35826=CARTESIAN_POINT('',(0.5,-6.82188856954009,5.8704204572397));
#35827=CARTESIAN_POINT('Origin',(0.5,0.,0.));
#35828=CARTESIAN_POINT('',(0.5,-6.77949332160295,5.68867034572587));
#35829=CARTESIAN_POINT('Origin',(0.5,-6.77949332160295,5.68867034572587));
#35830=CARTESIAN_POINT('',(11.,-6.82188856954009,5.8704204572397));
#35831=CARTESIAN_POINT('',(5.75,-6.82188856954009,5.8704204572397));
#35832=CARTESIAN_POINT('',(11.,-6.77949332160295,5.68867034572587));
#35833=CARTESIAN_POINT('Origin',(11.,-6.85609776591485,5.75294910669453));
#35834=CARTESIAN_POINT('Origin',(11.,0.,0.));
#35835=CARTESIAN_POINT('Origin',(0.5,-5.93213453413103,6.83628406877377));
#35836=CARTESIAN_POINT('',(11.,-5.8704204572397,6.82188856954009));
#35837=CARTESIAN_POINT('',(0.5,-5.8704204572397,6.82188856954009));
#35838=CARTESIAN_POINT('',(5.75,-5.8704204572397,6.82188856954009));
#35839=CARTESIAN_POINT('',(11.,-5.68867034572587,6.77949332160296));
#35840=CARTESIAN_POINT('',(11.,-5.93213453413103,6.83628406877377));
#35841=CARTESIAN_POINT('',(0.5,-5.68867034572587,6.77949332160296));
#35842=CARTESIAN_POINT('',(0.5,-5.68867034572587,6.77949332160296));
#35843=CARTESIAN_POINT('',(0.5,-5.93213453413103,6.83628406877377));
#35844=CARTESIAN_POINT('Origin',(0.5,-5.75294910669453,6.85609776591485));
#35845=CARTESIAN_POINT('',(0.5,-5.6988609389301,6.96584409807862));
#35846=CARTESIAN_POINT('Origin',(0.5,0.,0.));
#35847=CARTESIAN_POINT('',(0.5,-5.68867034572587,6.77949332160296));
#35848=CARTESIAN_POINT('Origin',(0.5,-5.68867034572587,6.77949332160296));
#35849=CARTESIAN_POINT('',(11.,-5.6988609389301,6.96584409807862));
#35850=CARTESIAN_POINT('',(5.75,-5.6988609389301,6.96584409807862));
#35851=CARTESIAN_POINT('',(11.,-5.68867034572587,6.77949332160296));
#35852=CARTESIAN_POINT('Origin',(11.,-5.75294910669453,6.85609776591485));
#35853=CARTESIAN_POINT('Origin',(11.,0.,0.));
#35854=CARTESIAN_POINT('Origin',(0.5,-4.65490381056766,7.76252990424917));
#35855=CARTESIAN_POINT('',(11.,-4.59662706138362,7.73763656800678));
#35856=CARTESIAN_POINT('',(0.5,-4.59662706138362,7.73763656800678));
#35857=CARTESIAN_POINT('',(5.75,-4.59662706138362,7.73763656800678));
#35858=CARTESIAN_POINT('',(11.,-4.425,7.66432482349228));
#35859=CARTESIAN_POINT('',(11.,-4.65490381056766,7.76252990424917));
#35860=CARTESIAN_POINT('',(0.5,-4.425,7.66432482349228));
#35861=CARTESIAN_POINT('',(0.5,-4.425,7.66432482349228));
#35862=CARTESIAN_POINT('',(0.5,-4.65490381056766,7.76252990424917));
#35863=CARTESIAN_POINT('Origin',(0.5,-4.475,7.75092736387073));
#35864=CARTESIAN_POINT('',(0.5,-4.4026763024535,7.84961409088462));
#35865=CARTESIAN_POINT('Origin',(0.5,0.,0.));
#35866=CARTESIAN_POINT('',(0.5,-4.425,7.66432482349228));
#35867=CARTESIAN_POINT('Origin',(0.5,-4.425,7.66432482349228));
#35868=CARTESIAN_POINT('',(11.,-4.4026763024535,7.84961409088462));
#35869=CARTESIAN_POINT('',(5.75,-4.4026763024535,7.84961409088462));
#35870=CARTESIAN_POINT('',(11.,-4.425,7.66432482349228));
#35871=CARTESIAN_POINT('Origin',(11.,-4.475,7.75092736387073));
#35872=CARTESIAN_POINT('Origin',(11.,0.,0.));
#35873=CARTESIAN_POINT('Origin',(0.5,-3.23623619021519,8.45291519661362));
#35874=CARTESIAN_POINT('',(11.,-3.18316747827294,8.41828039478761));
#35875=CARTESIAN_POINT('',(0.5,-3.18316747827294,8.41828039478761));
#35876=CARTESIAN_POINT('',(5.75,-3.18316747827294,8.41828039478761));
#35877=CARTESIAN_POINT('',(11.,-3.02687826843217,8.31627969395529));
#35878=CARTESIAN_POINT('',(11.,-3.23623619021519,8.45291519661362));
#35879=CARTESIAN_POINT('',(0.5,-3.02687826843217,8.31627969395529));
#35880=CARTESIAN_POINT('',(0.5,-3.02687826843217,8.31627969395529));
#35881=CARTESIAN_POINT('',(0.5,-3.23623619021519,8.45291519661362));
#35882=CARTESIAN_POINT('Origin',(0.5,-3.06108028276473,8.41024895603388));
#35883=CARTESIAN_POINT('',(0.5,-2.97271857438855,8.49487753163548));
#35884=CARTESIAN_POINT('Origin',(0.5,0.,0.));
#35885=CARTESIAN_POINT('',(0.5,-3.02687826843217,8.31627969395529));
#35886=CARTESIAN_POINT('Origin',(0.5,-3.02687826843217,8.31627969395529));
#35887=CARTESIAN_POINT('',(11.,-2.97271857438855,8.49487753163548));
#35888=CARTESIAN_POINT('',(5.75,-2.97271857438855,8.49487753163548));
#35889=CARTESIAN_POINT('',(11.,-3.02687826843217,8.31627969395529));
#35890=CARTESIAN_POINT('Origin',(11.,-3.06108028276473,8.41024895603388));
#35891=CARTESIAN_POINT('Origin',(11.,0.,0.));
#35892=CARTESIAN_POINT('Origin',(0.5,-1.71923717083755,8.88646293811044));
#35893=CARTESIAN_POINT('',(11.,-1.67298896209539,8.84313903162825));
#35894=CARTESIAN_POINT('',(0.5,-1.67298896209539,8.84313903162825));
#35895=CARTESIAN_POINT('',(5.75,-1.67298896209539,8.84313903162825));
#35896=CARTESIAN_POINT('',(11.,-1.53678637235233,8.71554861415804));
#35897=CARTESIAN_POINT('',(11.,-1.71923717083755,8.88646293811044));
#35898=CARTESIAN_POINT('',(0.5,-1.53678637235233,8.71554861415804));
#35899=CARTESIAN_POINT('',(0.5,-1.53678637235233,8.71554861415804));
#35900=CARTESIAN_POINT('',(0.5,-1.71923717083755,8.88646293811044));
#35901=CARTESIAN_POINT('Origin',(0.5,-1.55415119011903,8.81402938945926));
#35902=CARTESIAN_POINT('',(0.5,-1.45243629670899,8.88202841720304));
#35903=CARTESIAN_POINT('Origin',(0.5,0.,0.));
#35904=CARTESIAN_POINT('',(0.5,-1.53678637235233,8.71554861415804));
#35905=CARTESIAN_POINT('Origin',(0.5,-1.53678637235233,8.71554861415804));
#35906=CARTESIAN_POINT('',(11.,-1.45243629670899,8.88202841720304));
#35907=CARTESIAN_POINT('',(5.75,-1.45243629670899,8.88202841720304));
#35908=CARTESIAN_POINT('',(11.,-1.53678637235233,8.71554861415804));
#35909=CARTESIAN_POINT('Origin',(11.,-1.55415119011903,8.81402938945926));
#35910=CARTESIAN_POINT('Origin',(11.,0.,0.));
#35911=CARTESIAN_POINT('Origin',(0.5,-0.149999999999999,9.05));
#35912=CARTESIAN_POINT('',(11.,-0.111977522877842,8.99930336383712));
#35913=CARTESIAN_POINT('',(0.5,-0.111977522877842,8.99930336383712));
#35914=CARTESIAN_POINT('',(5.75,-0.111977522877842,8.99930336383712));
#35915=CARTESIAN_POINT('',(11.,5.41906208622704E-16,8.85));
#35916=CARTESIAN_POINT('',(11.,-0.149999999999999,9.05));
#35917=CARTESIAN_POINT('',(0.5,5.41906208622704E-16,8.85));
#35918=CARTESIAN_POINT('',(0.5,5.41906208622704E-16,8.85));
#35919=CARTESIAN_POINT('',(0.5,-0.149999999999999,9.05));
#35920=CARTESIAN_POINT('Origin',(0.5,5.48029442618441E-16,8.95));
#35921=CARTESIAN_POINT('',(0.5,0.111977522877842,8.99930336383712));
#35922=CARTESIAN_POINT('Origin',(0.5,0.,0.));
#35923=CARTESIAN_POINT('',(0.5,5.41906208622704E-16,8.85));
#35924=CARTESIAN_POINT('Origin',(0.5,5.41906208622704E-16,8.85));
#35925=CARTESIAN_POINT('',(11.,0.111977522877842,8.99930336383712));
#35926=CARTESIAN_POINT('',(5.75,0.111977522877842,8.99930336383712));
#35927=CARTESIAN_POINT('',(11.,5.41906208622704E-16,8.85));
#35928=CARTESIAN_POINT('Origin',(11.,5.48029442618441E-16,8.95));
#35929=CARTESIAN_POINT('Origin',(11.,0.,0.));
#35930=CARTESIAN_POINT('Origin',(0.5,1.42379484493389,8.93855739141052));
#35931=CARTESIAN_POINT('',(11.,1.45243629670899,8.88202841720304));
#35932=CARTESIAN_POINT('',(0.500000000000002,1.45243629670899,8.88202841720304));
#35933=CARTESIAN_POINT('',(5.75,1.45243629670899,8.88202841720304));
#35934=CARTESIAN_POINT('',(11.,1.53678637235233,8.71554861415804));
#35935=CARTESIAN_POINT('',(11.,1.42379484493389,8.93855739141052));
#35936=CARTESIAN_POINT('',(0.5,1.53678637235233,8.71554861415804));
#35937=CARTESIAN_POINT('',(0.5,1.53678637235233,8.71554861415804));
#35938=CARTESIAN_POINT('',(0.5,1.42379484493389,8.93855739141052));
#35939=CARTESIAN_POINT('Origin',(0.5,1.55415119011903,8.81402938945926));
#35940=CARTESIAN_POINT('',(0.5,1.67298896209539,8.84313903162825));
#35941=CARTESIAN_POINT('Origin',(0.5,0.,0.));
#35942=CARTESIAN_POINT('',(0.5,1.53678637235233,8.71554861415804));
#35943=CARTESIAN_POINT('Origin',(0.5,1.53678637235233,8.71554861415804));
#35944=CARTESIAN_POINT('',(11.,1.67298896209539,8.84313903162825));
#35945=CARTESIAN_POINT('',(5.75,1.67298896209539,8.84313903162825));
#35946=CARTESIAN_POINT('',(11.,1.53678637235233,8.71554861415804));
#35947=CARTESIAN_POINT('Origin',(11.,1.55415119011903,8.81402938945926));
#35948=CARTESIAN_POINT('Origin',(11.,0.,0.));
#35949=CARTESIAN_POINT('Origin',(0.5,2.95432840397942,8.55552123961132));
#35950=CARTESIAN_POINT('',(11.,2.97271857438855,8.49487753163548));
#35951=CARTESIAN_POINT('',(0.5,2.97271857438855,8.49487753163548));
#35952=CARTESIAN_POINT('',(5.75,2.97271857438855,8.49487753163548));
#35953=CARTESIAN_POINT('',(11.,3.02687826843217,8.31627969395529));
#35954=CARTESIAN_POINT('',(11.,2.95432840397942,8.55552123961132));
#35955=CARTESIAN_POINT('',(0.5,3.02687826843217,8.31627969395529));
#35956=CARTESIAN_POINT('',(0.5,3.02687826843217,8.31627969395529));
#35957=CARTESIAN_POINT('',(0.5,2.95432840397942,8.55552123961132));
#35958=CARTESIAN_POINT('Origin',(0.5,3.06108028276474,8.41024895603388));
#35959=CARTESIAN_POINT('',(0.5,3.18316747827294,8.41828039478761));
#35960=CARTESIAN_POINT('Origin',(0.5,0.,0.));
#35961=CARTESIAN_POINT('',(0.5,3.02687826843217,8.31627969395529));
#35962=CARTESIAN_POINT('Origin',(0.5,3.02687826843217,8.31627969395529));
#35963=CARTESIAN_POINT('',(11.,3.18316747827294,8.41828039478761));
#35964=CARTESIAN_POINT('',(5.75,3.18316747827294,8.41828039478761));
#35965=CARTESIAN_POINT('',(11.,3.02687826843217,8.31627969395529));
#35966=CARTESIAN_POINT('Origin',(11.,3.06108028276474,8.41024895603388));
#35967=CARTESIAN_POINT('Origin',(11.,0.,0.));
#35968=CARTESIAN_POINT('Origin',(0.5,4.39509618943234,7.91252990424917));
#35969=CARTESIAN_POINT('',(11.,4.4026763024535,7.84961409088462));
#35970=CARTESIAN_POINT('',(0.5,4.4026763024535,7.84961409088462));
#35971=CARTESIAN_POINT('',(5.75,4.4026763024535,7.84961409088462));
#35972=CARTESIAN_POINT('',(11.,4.425,7.66432482349228));
#35973=CARTESIAN_POINT('',(11.,4.39509618943234,7.91252990424917));
#35974=CARTESIAN_POINT('',(0.5,4.425,7.66432482349228));
#35975=CARTESIAN_POINT('',(0.5,4.425,7.66432482349228));
#35976=CARTESIAN_POINT('',(0.5,4.39509618943234,7.91252990424917));
#35977=CARTESIAN_POINT('Origin',(0.5,4.475,7.75092736387073));
#35978=CARTESIAN_POINT('',(0.5,4.59662706138363,7.73763656800678));
#35979=CARTESIAN_POINT('Origin',(0.5,0.,0.));
#35980=CARTESIAN_POINT('',(0.5,4.425,7.66432482349228));
#35981=CARTESIAN_POINT('Origin',(0.5,4.425,7.66432482349228));
#35982=CARTESIAN_POINT('',(11.,4.59662706138363,7.73763656800678));
#35983=CARTESIAN_POINT('',(5.75,4.59662706138363,7.73763656800678));
#35984=CARTESIAN_POINT('',(11.,4.425,7.66432482349228));
#35985=CARTESIAN_POINT('Origin',(11.,4.475,7.75092736387073));
#35986=CARTESIAN_POINT('Origin',(11.,0.,0.));
#35987=CARTESIAN_POINT('Origin',(0.5,5.70232120119534,7.02912035167973));
#35988=CARTESIAN_POINT('',(11.,5.6988609389301,6.96584409807862));
#35989=CARTESIAN_POINT('',(0.5,5.6988609389301,6.96584409807862));
#35990=CARTESIAN_POINT('',(5.75,5.6988609389301,6.96584409807862));
#35991=CARTESIAN_POINT('',(11.,5.68867034572587,6.77949332160296));
#35992=CARTESIAN_POINT('',(11.,5.70232120119534,7.02912035167973));
#35993=CARTESIAN_POINT('',(0.5,5.68867034572587,6.77949332160296));
#35994=CARTESIAN_POINT('',(0.5,5.68867034572587,6.77949332160296));
#35995=CARTESIAN_POINT('',(0.5,5.70232120119534,7.02912035167973));
#35996=CARTESIAN_POINT('Origin',(0.5,5.75294910669453,6.85609776591485));
#35997=CARTESIAN_POINT('',(0.5,5.8704204572397,6.82188856954009));
#35998=CARTESIAN_POINT('Origin',(0.5,0.,0.));
#35999=CARTESIAN_POINT('',(0.5,5.68867034572587,6.77949332160296));
#36000=CARTESIAN_POINT('Origin',(0.5,5.68867034572587,6.77949332160296));
#36001=CARTESIAN_POINT('',(11.,5.8704204572397,6.82188856954009));
#36002=CARTESIAN_POINT('',(5.75,5.8704204572397,6.82188856954009));
#36003=CARTESIAN_POINT('',(11.,5.68867034572587,6.77949332160296));
#36004=CARTESIAN_POINT('Origin',(11.,5.75294910669453,6.85609776591485));
#36005=CARTESIAN_POINT('Origin',(11.,0.,0.));
#36006=CARTESIAN_POINT('Origin',(0.5,6.83628406877377,5.93213453413103));
#36007=CARTESIAN_POINT('',(11.,6.82188856954009,5.8704204572397));
#36008=CARTESIAN_POINT('',(0.500000000000002,6.82188856954009,5.8704204572397));
#36009=CARTESIAN_POINT('',(5.75,6.82188856954009,5.8704204572397));
#36010=CARTESIAN_POINT('',(11.,6.77949332160296,5.68867034572587));
#36011=CARTESIAN_POINT('',(11.,6.83628406877377,5.93213453413103));
#36012=CARTESIAN_POINT('',(0.5,6.77949332160296,5.68867034572587));
#36013=CARTESIAN_POINT('',(0.5,6.77949332160296,5.68867034572587));
#36014=CARTESIAN_POINT('',(0.5,6.83628406877377,5.93213453413103));
#36015=CARTESIAN_POINT('Origin',(0.5,6.85609776591486,5.75294910669453));
#36016=CARTESIAN_POINT('',(0.5,6.96584409807862,5.6988609389301));
#36017=CARTESIAN_POINT('Origin',(0.5,0.,0.));
#36018=CARTESIAN_POINT('',(0.5,6.77949332160296,5.68867034572587));
#36019=CARTESIAN_POINT('Origin',(0.5,6.77949332160296,5.68867034572587));
#36020=CARTESIAN_POINT('',(11.,6.96584409807862,5.6988609389301));
#36021=CARTESIAN_POINT('',(5.75,6.96584409807862,5.6988609389301));
#36022=CARTESIAN_POINT('',(11.,6.77949332160296,5.68867034572587));
#36023=CARTESIAN_POINT('Origin',(11.,6.85609776591486,5.75294910669453));
#36024=CARTESIAN_POINT('Origin',(11.,0.,0.));
#36025=CARTESIAN_POINT('Origin',(0.5,7.76252990424917,4.65490381056767));
#36026=CARTESIAN_POINT('',(11.,7.73763656800678,4.59662706138362));
#36027=CARTESIAN_POINT('',(0.5,7.73763656800678,4.59662706138362));
#36028=CARTESIAN_POINT('',(5.75,7.73763656800678,4.59662706138362));
#36029=CARTESIAN_POINT('',(11.,7.66432482349228,4.425));
#36030=CARTESIAN_POINT('',(11.,7.76252990424917,4.65490381056767));
#36031=CARTESIAN_POINT('',(0.5,7.66432482349228,4.425));
#36032=CARTESIAN_POINT('',(0.5,7.66432482349228,4.425));
#36033=CARTESIAN_POINT('',(0.5,7.76252990424917,4.65490381056767));
#36034=CARTESIAN_POINT('Origin',(0.5,7.75092736387073,4.475));
#36035=CARTESIAN_POINT('',(0.5,7.84961409088462,4.4026763024535));
#36036=CARTESIAN_POINT('Origin',(0.5,0.,0.));
#36037=CARTESIAN_POINT('',(0.5,7.66432482349228,4.425));
#36038=CARTESIAN_POINT('Origin',(0.5,7.66432482349228,4.425));
#36039=CARTESIAN_POINT('',(11.,7.84961409088462,4.4026763024535));
#36040=CARTESIAN_POINT('',(5.75,7.84961409088462,4.4026763024535));
#36041=CARTESIAN_POINT('',(11.,7.66432482349228,4.425));
#36042=CARTESIAN_POINT('Origin',(11.,7.75092736387073,4.475));
#36043=CARTESIAN_POINT('Origin',(11.,0.,0.));
#36044=CARTESIAN_POINT('Origin',(0.5,8.45291519661362,3.23623619021519));
#36045=CARTESIAN_POINT('',(11.,8.41828039478761,3.18316747827294));
#36046=CARTESIAN_POINT('',(0.5,8.41828039478761,3.18316747827294));
#36047=CARTESIAN_POINT('',(5.75,8.41828039478761,3.18316747827294));
#36048=CARTESIAN_POINT('',(11.,8.31627969395529,3.02687826843217));
#36049=CARTESIAN_POINT('',(11.,8.45291519661362,3.23623619021519));
#36050=CARTESIAN_POINT('',(0.5,8.31627969395529,3.02687826843217));
#36051=CARTESIAN_POINT('',(0.5,8.31627969395529,3.02687826843217));
#36052=CARTESIAN_POINT('',(0.5,8.45291519661362,3.23623619021519));
#36053=CARTESIAN_POINT('Origin',(0.5,8.41024895603388,3.06108028276473));
#36054=CARTESIAN_POINT('',(0.5,8.49487753163548,2.97271857438855));
#36055=CARTESIAN_POINT('Origin',(0.5,0.,0.));
#36056=CARTESIAN_POINT('',(0.5,8.31627969395529,3.02687826843217));
#36057=CARTESIAN_POINT('Origin',(0.5,8.31627969395529,3.02687826843217));
#36058=CARTESIAN_POINT('',(11.,8.49487753163548,2.97271857438855));
#36059=CARTESIAN_POINT('',(5.75,8.49487753163548,2.97271857438855));
#36060=CARTESIAN_POINT('',(11.,8.31627969395529,3.02687826843217));
#36061=CARTESIAN_POINT('Origin',(11.,8.41024895603388,3.06108028276473));
#36062=CARTESIAN_POINT('Origin',(11.,0.,0.));
#36063=CARTESIAN_POINT('Origin',(0.5,8.88646293811044,1.71923717083755));
#36064=CARTESIAN_POINT('',(11.,8.84313903162825,1.67298896209539));
#36065=CARTESIAN_POINT('',(0.5,8.84313903162825,1.67298896209539));
#36066=CARTESIAN_POINT('',(5.75,8.84313903162825,1.67298896209539));
#36067=CARTESIAN_POINT('',(11.,8.71554861415804,1.53678637235233));
#36068=CARTESIAN_POINT('',(11.,8.88646293811044,1.71923717083755));
#36069=CARTESIAN_POINT('',(0.5,8.71554861415804,1.53678637235233));
#36070=CARTESIAN_POINT('',(0.5,8.71554861415804,1.53678637235233));
#36071=CARTESIAN_POINT('',(0.5,8.88646293811044,1.71923717083755));
#36072=CARTESIAN_POINT('Origin',(0.5,8.81402938945926,1.55415119011903));
#36073=CARTESIAN_POINT('',(0.5,8.88202841720304,1.45243629670899));
#36074=CARTESIAN_POINT('Origin',(0.5,0.,0.));
#36075=CARTESIAN_POINT('',(0.5,8.71554861415804,1.53678637235233));
#36076=CARTESIAN_POINT('Origin',(0.5,8.71554861415804,1.53678637235233));
#36077=CARTESIAN_POINT('',(11.,8.88202841720304,1.45243629670899));
#36078=CARTESIAN_POINT('',(5.75,8.88202841720304,1.45243629670899));
#36079=CARTESIAN_POINT('',(11.,8.71554861415804,1.53678637235233));
#36080=CARTESIAN_POINT('Origin',(11.,8.81402938945926,1.55415119011903));
#36081=CARTESIAN_POINT('Origin',(11.,0.,0.));
#36082=CARTESIAN_POINT('Origin',(0.5,9.05,0.15));
#36083=CARTESIAN_POINT('',(11.,8.99930336383712,0.111977522877842));
#36084=CARTESIAN_POINT('',(0.5,8.99930336383712,0.111977522877842));
#36085=CARTESIAN_POINT('',(5.75,8.99930336383712,0.111977522877842));
#36086=CARTESIAN_POINT('',(11.,8.85,0.));
#36087=CARTESIAN_POINT('',(11.,9.05,0.15));
#36088=CARTESIAN_POINT('',(0.5,8.85,0.));
#36089=CARTESIAN_POINT('',(0.5,8.85,0.));
#36090=CARTESIAN_POINT('',(0.5,9.05,0.15));
#36091=CARTESIAN_POINT('Origin',(0.5,8.95,0.));
#36092=CARTESIAN_POINT('',(0.5,8.99930336383712,-0.111977522877842));
#36093=CARTESIAN_POINT('Origin',(0.5,0.,0.));
#36094=CARTESIAN_POINT('',(0.5,8.85,0.));
#36095=CARTESIAN_POINT('Origin',(0.5,8.85,0.));
#36096=CARTESIAN_POINT('',(11.,8.99930336383712,-0.111977522877842));
#36097=CARTESIAN_POINT('',(5.75,8.99930336383712,-0.111977522877842));
#36098=CARTESIAN_POINT('',(11.,8.85,0.));
#36099=CARTESIAN_POINT('Origin',(11.,8.95,0.));
#36100=CARTESIAN_POINT('Origin',(11.,0.,0.));
#36101=CARTESIAN_POINT('Origin',(12.,0.,5.77350269189626));
#36102=CARTESIAN_POINT('',(12.,3.53525079574969E-16,5.77350269189626));
#36103=CARTESIAN_POINT('',(12.,5.,2.88675134594813));
#36104=CARTESIAN_POINT('',(12.,1.25,5.05181485540923));
#36105=CARTESIAN_POINT('',(6.,5.55111512312578E-16,5.77350269189626));
#36106=CARTESIAN_POINT('',(12.,3.53525079574969E-16,5.77350269189626));
#36107=CARTESIAN_POINT('',(6.,5.,2.88675134594813));
#36108=CARTESIAN_POINT('',(6.,5.,2.88675134594813));
#36109=CARTESIAN_POINT('',(12.,5.,2.88675134594813));
#36110=CARTESIAN_POINT('Origin',(12.,-5.,2.88675134594813));
#36111=CARTESIAN_POINT('',(12.,-5.,2.88675134594813));
#36112=CARTESIAN_POINT('',(12.,-3.75,3.60843918243516));
#36113=CARTESIAN_POINT('',(6.,-5.,2.88675134594813));
#36114=CARTESIAN_POINT('',(12.,-5.,2.88675134594813));
#36115=CARTESIAN_POINT('',(6.,3.53525079574969E-16,5.77350269189626));
#36116=CARTESIAN_POINT('Origin',(12.,-5.,-2.88675134594813));
#36117=CARTESIAN_POINT('',(12.,-5.,-2.88675134594813));
#36118=CARTESIAN_POINT('',(12.,-5.,-1.44337567297407));
#36119=CARTESIAN_POINT('',(6.,-5.,-2.88675134594813));
#36120=CARTESIAN_POINT('',(12.,-5.,-2.88675134594813));
#36121=CARTESIAN_POINT('',(6.,-5.,2.88675134594813));
#36122=CARTESIAN_POINT('Origin',(12.,-1.11022302462516E-15,-5.77350269189626));
#36123=CARTESIAN_POINT('',(12.,-1.06057523872491E-15,-5.77350269189626));
#36124=CARTESIAN_POINT('',(12.,-1.25,-5.05181485540923));
#36125=CARTESIAN_POINT('',(6.,-1.11022302462516E-15,-5.77350269189626));
#36126=CARTESIAN_POINT('',(12.,-1.06057523872491E-15,-5.77350269189626));
#36127=CARTESIAN_POINT('',(6.,-5.,-2.88675134594813));
#36128=CARTESIAN_POINT('Origin',(12.,5.,-2.88675134594813));
#36129=CARTESIAN_POINT('',(12.,5.,-2.88675134594813));
#36130=CARTESIAN_POINT('',(12.,3.75,-3.60843918243516));
#36131=CARTESIAN_POINT('',(6.,5.,-2.88675134594813));
#36132=CARTESIAN_POINT('',(12.,5.,-2.88675134594813));
#36133=CARTESIAN_POINT('',(6.,-1.06057523872491E-15,-5.77350269189626));
#36134=CARTESIAN_POINT('Origin',(12.,5.,2.88675134594813));
#36135=CARTESIAN_POINT('',(12.,5.,1.44337567297406));
#36136=CARTESIAN_POINT('',(6.,5.,-2.88675134594813));
#36137=CARTESIAN_POINT('Origin',(6.,0.,0.));
#36138=CARTESIAN_POINT('Origin',(-60.,5.5,0.));
#36139=CARTESIAN_POINT('',(-60.,-5.5,-6.73555739531044E-16));
#36140=CARTESIAN_POINT('Origin',(-60.,0.,0.));
#36141=CARTESIAN_POINT('Origin',(-59.75,0.,0.));
#36142=CARTESIAN_POINT('',(-59.75,-5.75,-7.04171909509728E-16));
#36143=CARTESIAN_POINT('Origin',(-29.75,0.,0.));
#36144=CARTESIAN_POINT('Origin',(0.,0.,0.));
#36145=CARTESIAN_POINT('Origin',(0.,9.,0.));
#36146=CARTESIAN_POINT('',(0.,-9.,-1.10218211923262E-15));
#36147=CARTESIAN_POINT('Origin',(0.,0.,0.));
#36148=CARTESIAN_POINT('Origin',(5.75,0.,0.));
#36149=CARTESIAN_POINT('',(11.5,-9.,-1.10218211923262E-15));
#36150=CARTESIAN_POINT('Origin',(11.5,0.,0.));
#36151=CARTESIAN_POINT('',(5.75,-9.,-1.10218211923262E-15));
#36152=CARTESIAN_POINT('',(5.75,-9.,-1.10218211923262E-15));
#36153=CARTESIAN_POINT('Origin',(11.75,0.,0.));
#36154=CARTESIAN_POINT('',(12.,-8.5,-1.04094977927525E-15));
#36155=CARTESIAN_POINT('Origin',(12.,0.,0.));
#36156=CARTESIAN_POINT('',(11.75,-8.75,-1.07156594925393E-15));
#36157=CARTESIAN_POINT('Origin',(12.,0.,0.));
#36158=CARTESIAN_POINT('',(0.,0.,0.));
#36159=CARTESIAN_POINT('Origin',(-6.5,0.,0.));
#36160=CARTESIAN_POINT('',(-11.0923131746348,-8.92462941051898,0.000191549954296211));
#36161=CARTESIAN_POINT('',(-11.3076868253652,-8.92481439709363,0.000136450195849817));
#36162=CARTESIAN_POINT('',(-6.5,-8.925,-1.09299726823901E-15));
#36163=CARTESIAN_POINT('',(-11.575,3.89083931480654,8.03230655290357));
#36164=CARTESIAN_POINT('Ctrl Pts',(-11.0923131746348,-8.92462941051898,
0.000191549954296211));
#36165=CARTESIAN_POINT('Ctrl Pts',(-11.1048718995935,-8.92500789246107,
0.469746294508158));
#36166=CARTESIAN_POINT('Ctrl Pts',(-11.1174306245523,-8.88857179765685,
0.939242703025031));
#36167=CARTESIAN_POINT('Ctrl Pts',(-11.1299893495111,-8.81480118765077,
1.40279733933406));
#36168=CARTESIAN_POINT('Ctrl Pts',(-11.1691356476798,-8.58485377619997,
2.8477249151872));
#36169=CARTESIAN_POINT('Ctrl Pts',(-11.2082819458485,-7.99216188082716,
4.23492186077868));
#36170=CARTESIAN_POINT('Ctrl Pts',(-11.2474282440173,-7.10700456064237,
5.39990921955463));
#36171=CARTESIAN_POINT('Ctrl Pts',(-11.286574542186,-6.22184724045757,6.56489657833059));
#36172=CARTESIAN_POINT('Ctrl Pts',(-11.3257208403548,-5.0442244954608,7.507674350291));
#36173=CARTESIAN_POINT('Ctrl Pts',(-11.3648671385235,-3.71377318840326,
8.11643476640391));
#36174=CARTESIAN_POINT('Ctrl Pts',(-11.4040134366923,-2.38332188134573,
8.72519518251681));
#36175=CARTESIAN_POINT('Ctrl Pts',(-11.443159734861,-0.90004201222745,8.99993824278221));
#36176=CARTESIAN_POINT('Ctrl Pts',(-11.4823060330297,0.560184619660341,
8.90812021137253));
#36177=CARTESIAN_POINT('Ctrl Pts',(-11.5132040220198,1.71273463091833,8.8356486711171));
#36178=CARTESIAN_POINT('Ctrl Pts',(-11.5441020110099,2.85092277360137,8.53481431262945));
#36179=CARTESIAN_POINT('Ctrl Pts',(-11.575,3.89095401968739,8.03231038431322));
#36180=CARTESIAN_POINT('',(-11.575,-3.89072460992591,8.03230272149381));
#36181=CARTESIAN_POINT('Origin',(-11.575,0.,0.));
#36182=CARTESIAN_POINT('Ctrl Pts',(-11.575,-3.89072460992591,8.03230272149381));
#36183=CARTESIAN_POINT('Ctrl Pts',(-11.5358537018313,-5.20782651162706,
7.39431870116846));
#36184=CARTESIAN_POINT('Ctrl Pts',(-11.4967074036625,-6.36443119534448,
6.42659434900291));
#36185=CARTESIAN_POINT('Ctrl Pts',(-11.4575611054938,-7.2237987510989,5.2426655805034));
#36186=CARTESIAN_POINT('Ctrl Pts',(-11.418414807325,-8.08316630685333,4.05873681200389));
#36187=CARTESIAN_POINT('Ctrl Pts',(-11.3792685091563,-8.64529673464475,
2.65860362717041));
#36188=CARTESIAN_POINT('Ctrl Pts',(-11.3401222109875,-8.84347878979323,
1.20890931115065));
#36189=CARTESIAN_POINT('Ctrl Pts',(-11.3293104157801,-8.89821458587845,
0.808519011392666));
#36190=CARTESIAN_POINT('Ctrl Pts',(-11.3184986205726,-8.92518817393498,
0.404348157749692));
#36191=CARTESIAN_POINT('Ctrl Pts',(-11.3076868253652,-8.92481439709363,
0.000136450195849817));
#36192=CARTESIAN_POINT('Origin',(-6.5,0.,0.));
#36193=CARTESIAN_POINT('',(-9.59231317463479,-8.92556073748128,0.000127033491416559));
#36194=CARTESIAN_POINT('',(-9.80768682536521,-8.92567539102041,7.01672918444194E-5));
#36195=CARTESIAN_POINT('',(-6.5,-8.925,-1.09299726823901E-15));
#36196=CARTESIAN_POINT('Ctrl Pts',(-9.59231317463479,-8.92556073748128,
0.000127033491416559));
#36197=CARTESIAN_POINT('Ctrl Pts',(-9.59597002339987,-8.92565700983877,
0.136810759713388));
#36198=CARTESIAN_POINT('Ctrl Pts',(-9.59962687216495,-8.92258036831299,
0.273490150281187));
#36199=CARTESIAN_POINT('Ctrl Pts',(-9.60328372093003,-8.91630184308366,
0.410022300018877));
#36200=CARTESIAN_POINT('Ctrl Pts',(-9.64243001909878,-8.8490906904009,1.87158896208352));
#36201=CARTESIAN_POINT('Ctrl Pts',(-9.68157631726752,-8.41495821228372,
3.31628249397104));
#36202=CARTESIAN_POINT('Ctrl Pts',(-9.72072261543627,-7.66538193801836,
4.57279745790092));
#36203=CARTESIAN_POINT('Ctrl Pts',(-9.75986891360501,-6.91580566375299,
5.8293124218308));
#36204=CARTESIAN_POINT('Ctrl Pts',(-9.79901521177375,-5.85078559333945,
6.89764881780305));
#36205=CARTESIAN_POINT('Ctrl Pts',(-9.83816150994249,-4.59660714585951,
7.65112799401389));
#36206=CARTESIAN_POINT('Ctrl Pts',(-9.87730780811124,-3.34242869837957,
8.40460717022472));
#36207=CARTESIAN_POINT('Ctrl Pts',(-9.91645410627998,-1.89909187383322,
8.84322912667415));
#36208=CARTESIAN_POINT('Ctrl Pts',(-9.95560040444873,-0.437741236130637,
8.91498398627114));
#36209=CARTESIAN_POINT('Ctrl Pts',(-9.99474670261747,1.02360940157195,8.98673884586812));
#36210=CARTESIAN_POINT('Ctrl Pts',(-10.0338930007862,2.50297385243078,8.69162660861266));
#36211=CARTESIAN_POINT('Ctrl Pts',(-10.073039298955,3.82493555385304,8.06464040206903));
#36212=CARTESIAN_POINT('Ctrl Pts',(-10.1121855971237,5.14689725527529,7.4376541955254));
#36213=CARTESIAN_POINT('Ctrl Pts',(-10.1513318952925,6.31145620726098,6.4787940196936));
#36214=CARTESIAN_POINT('Ctrl Pts',(-10.1904781934612,7.18052410640066,5.30175729819094));
#36215=CARTESIAN_POINT('Ctrl Pts',(-10.2296244916299,8.04959200554035,4.12472057668828));
#36216=CARTESIAN_POINT('Ctrl Pts',(-10.2687707897987,8.62316885183402,2.72950730951476));
#36217=CARTESIAN_POINT('Ctrl Pts',(-10.3079170879674,8.83324241194816,1.28155581867923));
#36218=CARTESIAN_POINT('Ctrl Pts',(-10.3470633861362,9.0433159720623,-0.166395672156314));
#36219=CARTESIAN_POINT('Ctrl Pts',(-10.3862096843049,8.8898862459969,-1.66708538665386));
#36220=CARTESIAN_POINT('Ctrl Pts',(-10.4253559824737,8.39114626135687,-3.0425681824554));
#36221=CARTESIAN_POINT('Ctrl Pts',(-10.4645022806424,7.89240627671684,-4.41805097825693));
#36222=CARTESIAN_POINT('Ctrl Pts',(-10.5036485788111,7.04835603350219,-5.66832685536245));
#36223=CARTESIAN_POINT('Ctrl Pts',(-10.5427948769799,5.95907931141562,-6.64514342149727));
#36224=CARTESIAN_POINT('Ctrl Pts',(-10.5819411751486,4.86980258932905,-7.62195998763208));
#36225=CARTESIAN_POINT('Ctrl Pts',(-10.6210874733174,3.53529938837056,-8.32531724279619));
#36226=CARTESIAN_POINT('Ctrl Pts',(-10.6602337714861,2.11380926617132,-8.6718144581943));
#36227=CARTESIAN_POINT('Ctrl Pts',(-10.6993800696549,0.692319143972085,
-9.01831167359242));
#36228=CARTESIAN_POINT('Ctrl Pts',(-10.7385263678236,-0.816157899467901,
-9.00794884922453));
#36229=CARTESIAN_POINT('Ctrl Pts',(-10.7776726659923,-2.23275327449356,
-8.64195417971889));
#36230=CARTESIAN_POINT('Ctrl Pts',(-10.8168189641611,-3.6493486495192,-8.27595951021326));
#36231=CARTESIAN_POINT('Ctrl Pts',(-10.8559652623299,-4.97406235613052,
-7.55433299556987));
#36232=CARTESIAN_POINT('Ctrl Pts',(-10.8951115604986,-6.04981560800573,
-6.56264309955188));
#36233=CARTESIAN_POINT('Ctrl Pts',(-10.9342578586673,-7.12556885988095,
-5.57095320353389));
#36234=CARTESIAN_POINT('Ctrl Pts',(-10.9734041568361,-7.95236165702006,
-4.30919992614128));
#36235=CARTESIAN_POINT('Ctrl Pts',(-11.0125504550048,-8.43215659182522,
-2.92699418438758));
#36236=CARTESIAN_POINT('Ctrl Pts',(-11.0391380282148,-8.75802604951765,
-1.98822096522559));
#36237=CARTESIAN_POINT('Ctrl Pts',(-11.0657256014248,-8.92382814157034,
-0.9938839782484));
#36238=CARTESIAN_POINT('Ctrl Pts',(-11.0923131746348,-8.92462941051898,
0.000191549954296211));
#36239=CARTESIAN_POINT('Ctrl Pts',(-11.3076868253652,-8.92481439709363,
0.000136450195849817));
#36240=CARTESIAN_POINT('Ctrl Pts',(-11.2793523224039,-8.92383483904475,
-1.05918234052572));
#36241=CARTESIAN_POINT('Ctrl Pts',(-11.2510178194426,-8.73503129140792,
-2.11878171932437));
#36242=CARTESIAN_POINT('Ctrl Pts',(-11.2226833164813,-8.36587060142851,
-3.11135005349452));
#36243=CARTESIAN_POINT('Ctrl Pts',(-11.1835370183126,-7.85584667540975,
-4.48265965491388));
#36244=CARTESIAN_POINT('Ctrl Pts',(-11.1443907201438,-7.00156514086668,
-5.72602341054655));
#36245=CARTESIAN_POINT('Ctrl Pts',(-11.1052444219751,-5.90430480280725,
-6.69387629700437));
#36246=CARTESIAN_POINT('Ctrl Pts',(-11.0660981238063,-4.80704446474782,
-7.6617291834622));
#36247=CARTESIAN_POINT('Ctrl Pts',(-11.0269518256376,-3.46680532317205,
-8.35407120074516));
#36248=CARTESIAN_POINT('Ctrl Pts',(-10.9878055274688,-2.04251633415933,
-8.68887438049484));
#36249=CARTESIAN_POINT('Ctrl Pts',(-10.9486592293001,-0.618227345146618,
-9.02367756024451));
#36250=CARTESIAN_POINT('Ctrl Pts',(-10.9095129311313,0.890111491303043,
-9.00094190246089));
#36251=CARTESIAN_POINT('Ctrl Pts',(-10.8703666329626,2.30365266680068,-8.62332933535961));
#36252=CARTESIAN_POINT('Ctrl Pts',(-10.8312203347939,3.7171938422983,-8.24571676825833));
#36253=CARTESIAN_POINT('Ctrl Pts',(-10.7920740366251,5.03593735684391,-7.51322729183939));
#36254=CARTESIAN_POINT('Ctrl Pts',(-10.7529277384564,6.10350998281732,-6.51273355601827));
#36255=CARTESIAN_POINT('Ctrl Pts',(-10.7137814402876,7.17108260879073,-5.51223982019713));
#36256=CARTESIAN_POINT('Ctrl Pts',(-10.6746351421189,7.98748434619194,-4.24374182497381));
#36257=CARTESIAN_POINT('Ctrl Pts',(-10.6354888439501,8.45591106563375,-2.85764374611716));
#36258=CARTESIAN_POINT('Ctrl Pts',(-10.5963425457814,8.92433778507555,-1.47154566726051));
#36259=CARTESIAN_POINT('Ctrl Pts',(-10.5571962476126,9.04478948655795,0.0321524952294505));
#36260=CARTESIAN_POINT('Ctrl Pts',(-10.5180499494439,8.80298291682458,1.47514434110348));
#36261=CARTESIAN_POINT('Ctrl Pts',(-10.4789036512752,8.56117634709121,2.91813618697751));
#36262=CARTESIAN_POINT('Ctrl Pts',(-10.4397573531064,7.95711150614207,4.30042171623559));
#36263=CARTESIAN_POINT('Ctrl Pts',(-10.4006110549377,7.06241607297462,5.4580978224497));
#36264=CARTESIAN_POINT('Ctrl Pts',(-10.3614647567689,6.16772063980717,6.61577392866381));
#36265=CARTESIAN_POINT('Ctrl Pts',(-10.3223184586002,4.98239461442141,7.54884061183394));
#36266=CARTESIAN_POINT('Ctrl Pts',(-10.2831721604314,3.64698861005168,8.14665775885583));
#36267=CARTESIAN_POINT('Ctrl Pts',(-10.2440258622627,2.31158260568195,8.74447490587773));
#36268=CARTESIAN_POINT('Ctrl Pts',(-10.2048795640939,0.826096622328247,
9.00704251675139));
#36269=CARTESIAN_POINT('Ctrl Pts',(-10.1657332659252,-0.63332683218053,
8.90322705714482));
#36270=CARTESIAN_POINT('Ctrl Pts',(-10.1265869677565,-2.09275028668929,
8.79941159753826));
#36271=CARTESIAN_POINT('Ctrl Pts',(-10.0874406695877,-3.52611121235313,
8.32921306745147));
#36272=CARTESIAN_POINT('Ctrl Pts',(-10.048294371419,-4.76344798469274,7.54838525418809));
#36273=CARTESIAN_POINT('Ctrl Pts',(-10.0091480732502,-6.00078475703235,
6.76755744092469));
#36274=CARTESIAN_POINT('Ctrl Pts',(-9.97000177508148,-7.04209737604773,
5.67610034448468));
#36275=CARTESIAN_POINT('Ctrl Pts',(-9.93085547691274,-7.76391152766168,
4.40343432141847));
#36276=CARTESIAN_POINT('Ctrl Pts',(-9.89170917874399,-8.48572567927564,
3.13076829835225));
#36277=CARTESIAN_POINT('Ctrl Pts',(-9.85256288057525,-8.88804136348817,
1.67689334865984));
#36278=CARTESIAN_POINT('Ctrl Pts',(-9.81341658240651,-8.92315375777354,
0.214203524598343));
#36279=CARTESIAN_POINT('Ctrl Pts',(-9.81150666339274,-8.9248668655922,0.142839966946539));
#36280=CARTESIAN_POINT('Ctrl Pts',(-9.80959674437898,-8.92570588559066,
0.0714554264371891));
#36281=CARTESIAN_POINT('Ctrl Pts',(-9.80768682536521,-8.92567539102041,
7.01672918444194E-5));
#36282=CARTESIAN_POINT('Origin',(-6.5,0.,0.));
#36283=CARTESIAN_POINT('',(-8.09231317463479,-8.92541637255294,-0.000168493799423963));
#36284=CARTESIAN_POINT('',(-8.3076868253652,-8.92523072360173,-0.000199919135830939));
#36285=CARTESIAN_POINT('',(-6.5,-8.925,-1.09299726823901E-15));
#36286=CARTESIAN_POINT('Ctrl Pts',(-8.09231317463479,-8.92541637255294,
-0.000168493799423963));
#36287=CARTESIAN_POINT('Ctrl Pts',(-8.12621444537494,-8.9243130827288,1.26703437378749));
#36288=CARTESIAN_POINT('Ctrl Pts',(-8.16011571611509,-8.6515517834059,2.53469718746515));
#36289=CARTESIAN_POINT('Ctrl Pts',(-8.19401698685524,-8.12793759489029,
3.68852101759875));
#36290=CARTESIAN_POINT('Ctrl Pts',(-8.23316328502399,-7.52331255572497,
5.02085844042932));
#36291=CARTESIAN_POINT('Ctrl Pts',(-8.27230958319273,-6.58420875081621,
6.20140680939712));
#36292=CARTESIAN_POINT('Ctrl Pts',(-8.31145588136147,-5.42198099946788,
7.09018186544674));
#36293=CARTESIAN_POINT('Ctrl Pts',(-8.35060217953022,-4.25975324811955,
7.97895692149635));
#36294=CARTESIAN_POINT('Ctrl Pts',(-8.38974847769897,-2.87440155033164,
8.57595866462779));
#36295=CARTESIAN_POINT('Ctrl Pts',(-8.42889477586771,-1.43019484759195,
8.81039724085228));
#36296=CARTESIAN_POINT('Ctrl Pts',(-8.46804107403645,0.0140118551477458,
9.04483581707676));
#36297=CARTESIAN_POINT('Ctrl Pts',(-8.5071873722052,1.51707356283922,8.91671122639429));
#36298=CARTESIAN_POINT('Ctrl Pts',(-8.54633367037394,2.90076379616502,8.44121592204365));
#36299=CARTESIAN_POINT('Ctrl Pts',(-8.58547996854268,4.28445402949081,7.96572061769302));
#36300=CARTESIAN_POINT('Ctrl Pts',(-8.62462626671143,5.54877278845092,7.1428545996742));
#36301=CARTESIAN_POINT('Ctrl Pts',(-8.66377256488017,6.54380268775666,6.07018971922621));
#36302=CARTESIAN_POINT('Ctrl Pts',(-8.70291886304892,7.53883258706239,4.99752483877823));
#36303=CARTESIAN_POINT('Ctrl Pts',(-8.74206516121767,8.26457362671375,3.67506109590106));
#36304=CARTESIAN_POINT('Ctrl Pts',(-8.78121145938641,8.63497061035309,2.25961045360547));
#36305=CARTESIAN_POINT('Ctrl Pts',(-8.82035775755515,9.00536759399241,0.844159811309901));
#36306=CARTESIAN_POINT('Ctrl Pts',(-8.85950405572389,9.02042052161972,-0.664277730404096));
#36307=CARTESIAN_POINT('Ctrl Pts',(-8.89865035389264,8.67834448295411,-2.08683824933599));
#36308=CARTESIAN_POINT('Ctrl Pts',(-8.93779665206138,8.33626844428848,-3.5093987682679));
#36309=CARTESIAN_POINT('Ctrl Pts',(-8.97694295023013,7.63706343932992,-4.84608226441771));
#36310=CARTESIAN_POINT('Ctrl Pts',(-9.01608924839887,6.66363813757495,-5.93839065867938));
#36311=CARTESIAN_POINT('Ctrl Pts',(-9.05523554656762,5.69021283581997,-7.03069905294104));
#36312=CARTESIAN_POINT('Ctrl Pts',(-9.09438184473636,4.44256723726859,-7.87863234531457));
#36313=CARTESIAN_POINT('Ctrl Pts',(-9.1335281429051,3.06864169681512,-8.38164631683088));
#36314=CARTESIAN_POINT('Ctrl Pts',(-9.17267444107385,1.69471615636164,-8.8846602883472));
#36315=CARTESIAN_POINT('Ctrl Pts',(-9.21182073924259,0.19451067400608,-9.0427549390063));
#36316=CARTESIAN_POINT('Ctrl Pts',(-9.25096703741133,-1.254086949632,-8.83718409710341));
#36317=CARTESIAN_POINT('Ctrl Pts',(-9.29011333558007,-2.70268457327008,
-8.63161325520051));
#36318=CARTESIAN_POINT('Ctrl Pts',(-9.32925963374882,-4.09967433819068,
-8.06237692073562));
#36319=CARTESIAN_POINT('Ctrl Pts',(-9.36840593191757,-5.27940731184295,
-7.19697264687959));
#36320=CARTESIAN_POINT('Ctrl Pts',(-9.40755223008631,-6.45914028549521,
-6.33156837302357));
#36321=CARTESIAN_POINT('Ctrl Pts',(-9.44669852825506,-7.42161646787914,
-5.16999615977641));
#36322=CARTESIAN_POINT('Ctrl Pts',(-9.4858448264238,-8.05270964544695,-3.84999015703196));
#36323=CARTESIAN_POINT('Ctrl Pts',(-9.52133427582746,-8.62484929701108,
-2.65329242472025));
#36324=CARTESIAN_POINT('Ctrl Pts',(-9.55682372523113,-8.92462642130377,
-1.32637851751262));
#36325=CARTESIAN_POINT('Ctrl Pts',(-9.59231317463479,-8.92556073748128,
0.000127033491416559));
#36326=CARTESIAN_POINT('Ctrl Pts',(-9.80768682536521,-8.92567539102041,
7.01672918444194E-5));
#36327=CARTESIAN_POINT('Ctrl Pts',(-9.77045044621023,-8.92508085932995,
-1.39167919823139));
#36328=CARTESIAN_POINT('Ctrl Pts',(-9.73321406705525,-8.59397842659854,
-2.78370172177061));
#36329=CARTESIAN_POINT('Ctrl Pts',(-9.69597768790028,-7.9662589505002,-4.02582594453483));
#36330=CARTESIAN_POINT('Ctrl Pts',(-9.65683138973153,-7.30634264458328,
-5.33166089117597));
#36331=CARTESIAN_POINT('Ctrl Pts',(-9.61768509156279,-6.31860092839126,
-6.47182608602769));
#36332=CARTESIAN_POINT('Ctrl Pts',(-9.57853879339405,-5.12015589463028,
-7.31112574984834));
#36333=CARTESIAN_POINT('Ctrl Pts',(-9.5393924952253,-3.92171086086932,-8.15042541366897));
#36334=CARTESIAN_POINT('Ctrl Pts',(-9.50024619705655,-2.51256250953941,
-8.68885954645852));
#36335=CARTESIAN_POINT('Ctrl Pts',(-9.46109989888781,-1.05980148376962,
-8.86258297510901));
#36336=CARTESIAN_POINT('Ctrl Pts',(-9.42195360071907,0.392959542000176,
-9.03630640375949));
#36337=CARTESIAN_POINT('Ctrl Pts',(-9.38280730255033,1.88933324220986,-8.84531912827092));
#36338=CARTESIAN_POINT('Ctrl Pts',(-9.34366100438158,3.25188617149246,-8.31226758903612));
#36339=CARTESIAN_POINT('Ctrl Pts',(-9.30451470621284,4.61443910077506,-7.77921604980131));
#36340=CARTESIAN_POINT('Ctrl Pts',(-9.26536840804409,5.84317125913057,-6.90410024682028));
#36341=CARTESIAN_POINT('Ctrl Pts',(-9.22622210987535,6.79238496498866,-5.79068757957377));
#36342=CARTESIAN_POINT('Ctrl Pts',(-9.1870758117066,7.74159867084676,-4.67727491232726));
#36343=CARTESIAN_POINT('Ctrl Pts',(-9.14792951353786,8.41129392420744,-3.32556538081528));
#36344=CARTESIAN_POINT('Ctrl Pts',(-9.10878321536912,8.7220611925906,-1.89583878699597));
#36345=CARTESIAN_POINT('Ctrl Pts',(-9.06963691720037,9.03282846097377,-0.466112193176664));
#36346=CARTESIAN_POINT('Ctrl Pts',(-9.03049061903162,8.98466774437942,1.04163146294997));
#36347=CARTESIAN_POINT('Ctrl Pts',(-8.99134432086288,8.5832897299041,2.44861053777968));
#36348=CARTESIAN_POINT('Ctrl Pts',(-8.95219802269413,8.18191171542877,3.85558961260938));
#36349=CARTESIAN_POINT('Ctrl Pts',(-8.9130517245254,7.42731640307249,5.16180410614216));
#36350=CARTESIAN_POINT('Ctrl Pts',(-8.87390542635665,6.40898040252579,6.21236881989604));
#36351=CARTESIAN_POINT('Ctrl Pts',(-8.83475912818791,5.39064440197909,7.26293353364993));
#36352=CARTESIAN_POINT('Ctrl Pts',(-8.79561283001917,4.10856771324197,8.05784846762492));
#36353=CARTESIAN_POINT('Ctrl Pts',(-8.75646653185042,2.71477337922437,8.50285608797865));
#36354=CARTESIAN_POINT('Ctrl Pts',(-8.71732023368168,1.32097904520678,8.94786370833239));
#36355=CARTESIAN_POINT('Ctrl Pts',(-8.67817393551293,-0.184532934091295,
9.04296401506487));
#36356=CARTESIAN_POINT('Ctrl Pts',(-8.63902763734418,-1.62324553688074,
8.77688042991189));
#36357=CARTESIAN_POINT('Ctrl Pts',(-8.59988133917544,-3.06195813967019,
8.51079684475891));
#36358=CARTESIAN_POINT('Ctrl Pts',(-8.5607350410067,-4.43387136595102,7.88352936772046));
#36359=CARTESIAN_POINT('Ctrl Pts',(-8.52158874283795,-5.57630974936861,
6.96945663110273));
#36360=CARTESIAN_POINT('Ctrl Pts',(-8.48244244466921,-6.7187481327862,6.055383894485));
#36361=CARTESIAN_POINT('Ctrl Pts',(-8.44329614650046,-7.63171167334056,
4.85450589828798));
#36362=CARTESIAN_POINT('Ctrl Pts',(-8.40414984833172,-8.20694514987818,
3.50921749977058));
#36363=CARTESIAN_POINT('Ctrl Pts',(-8.37199550734288,-8.67943563347526,
2.4042123289676));
#36364=CARTESIAN_POINT('Ctrl Pts',(-8.33984116635404,-8.92406640251423,
1.20177635007904));
#36365=CARTESIAN_POINT('Ctrl Pts',(-8.3076868253652,-8.92523072360173,-0.000199919135830939));
#36366=CARTESIAN_POINT('Origin',(-6.5,0.,0.));
#36367=CARTESIAN_POINT('',(-6.59231317463479,-8.9244947065883,-0.000159621216041517));
#36368=CARTESIAN_POINT('',(-6.8076868253652,-8.92438047038815,-0.000115204162070208));
#36369=CARTESIAN_POINT('',(-6.5,-8.925,-1.09299726823901E-15));
#36370=CARTESIAN_POINT('Ctrl Pts',(-6.59231317463479,-8.9244947065883,-0.000159621216041517));
#36371=CARTESIAN_POINT('Ctrl Pts',(-6.61731256918127,-8.92387683722319,
0.934576087013297));
#36372=CARTESIAN_POINT('Ctrl Pts',(-6.64231196372775,-8.77761699705046,
1.86950071462885));
#36373=CARTESIAN_POINT('Ctrl Pts',(-6.66731135827423,-8.48888937989245,
2.75813595380074));
#36374=CARTESIAN_POINT('Ctrl Pts',(-6.70645765644297,-8.0367737348593,4.14964085489761));
#36375=CARTESIAN_POINT('Ctrl Pts',(-6.74560395461171,-7.23532553046888,
5.42764366535837));
#36376=CARTESIAN_POINT('Ctrl Pts',(-6.78475025278046,-6.17957698734988,
6.44060440495416));
#36377=CARTESIAN_POINT('Ctrl Pts',(-6.8238965509492,-5.12382844423088,7.45356514454996));
#36378=CARTESIAN_POINT('Ctrl Pts',(-6.86304284911794,-3.8137795623833,8.20148381328079));
#36379=CARTESIAN_POINT('Ctrl Pts',(-6.90218914728668,-2.404770204935,8.59567548859052));
#36380=CARTESIAN_POINT('Ctrl Pts',(-6.94133544545543,-0.995760847486707,
8.98986716390025));
#36381=CARTESIAN_POINT('Ctrl Pts',(-6.98048174362418,0.512208985562305,
9.03033184578887));
#36382=CARTESIAN_POINT('Ctrl Pts',(-7.01962804179292,1.94033083086948,8.71227140936716));
#36383=CARTESIAN_POINT('Ctrl Pts',(-7.05877433996167,3.36845267617666,8.39421097294545));
#36384=CARTESIAN_POINT('Ctrl Pts',(-7.09792063813041,4.71672653374201,7.7176254182134));
#36385=CARTESIAN_POINT('Ctrl Pts',(-7.13706693629915,5.82527999010435,6.76274129925055));
#36386=CARTESIAN_POINT('Ctrl Pts',(-7.1762132344679,6.93383344646669,5.8078571802877));
#36387=CARTESIAN_POINT('Ctrl Pts',(-7.21535953263664,7.80266650162602,4.57467449709404));
#36388=CARTESIAN_POINT('Ctrl Pts',(-7.25450583080539,8.32875673425172,3.20941865535734));
#36389=CARTESIAN_POINT('Ctrl Pts',(-7.29365212897413,8.85484696687742,1.84416281362066));
#36390=CARTESIAN_POINT('Ctrl Pts',(-7.33279842714287,9.03819437696948,0.346833813340936));
#36391=CARTESIAN_POINT('Ctrl Pts',(-7.37194472531162,8.85705843103853,-1.10502162552066));
#36392=CARTESIAN_POINT('Ctrl Pts',(-7.41109102348036,8.67592248510758,-2.55687706438227));
#36393=CARTESIAN_POINT('Ctrl Pts',(-7.4502373216491,8.13030318315361,-3.96325894182576));
#36394=CARTESIAN_POINT('Ctrl Pts',(-7.48938361981785,7.28489767416078,-5.15740464969601));
#36395=CARTESIAN_POINT('Ctrl Pts',(-7.52852991798659,6.43949216516796,-6.35155035756625));
#36396=CARTESIAN_POINT('Ctrl Pts',(-7.56767621615533,5.29430044913628,-7.33345989586326));
#36397=CARTESIAN_POINT('Ctrl Pts',(-7.60682251432408,3.98511434795003,-7.98670272875245));
#36398=CARTESIAN_POINT('Ctrl Pts',(-7.64596881249282,2.67592824676378,-8.63994556164165));
#36399=CARTESIAN_POINT('Ctrl Pts',(-7.68511511066157,1.20274776042295,-8.96452168912302));
#36400=CARTESIAN_POINT('Ctrl Pts',(-7.72426140883031,-0.259743816210902,
-8.92194429447076));
#36401=CARTESIAN_POINT('Ctrl Pts',(-7.76340770699906,-1.72223539284475,
-8.87936689981849));
#36402=CARTESIAN_POINT('Ctrl Pts',(-7.8025540051678,-3.17403805977162,-8.46963598303259));
#36403=CARTESIAN_POINT('Ctrl Pts',(-7.84170030333655,-4.44300341039844,
-7.74133564308426));
#36404=CARTESIAN_POINT('Ctrl Pts',(-7.88084660150529,-5.71196876102527,
-7.01303530313593));
#36405=CARTESIAN_POINT('Ctrl Pts',(-7.91999289967403,-6.79809679535206,
-5.96616554002517));
#36406=CARTESIAN_POINT('Ctrl Pts',(-7.95913919784278,-7.57259920438554,
-4.7248595887538));
#36407=CARTESIAN_POINT('Ctrl Pts',(-7.99828549601152,-8.34710161341902,
-3.48355363748243));
#36408=CARTESIAN_POINT('Ctrl Pts',(-8.03743179418027,-8.80997839715919,
-2.04781149805045));
#36409=CARTESIAN_POINT('Ctrl Pts',(-8.07657809234901,-8.90634365231834,
-0.587877189987794));
#36410=CARTESIAN_POINT('Ctrl Pts',(-8.08182311977761,-8.91925517729305,
-0.392267493849314));
#36411=CARTESIAN_POINT('Ctrl Pts',(-8.0870681472062,-8.92558706778834,-0.196223498611237));
#36412=CARTESIAN_POINT('Ctrl Pts',(-8.09231317463479,-8.92541637255294,
-0.000168493799423963));
#36413=CARTESIAN_POINT('Ctrl Pts',(-8.3076868253652,-8.92523072360173,-0.000199919135830939));
#36414=CARTESIAN_POINT('Ctrl Pts',(-8.3006948681853,-8.92548390506766,-0.261569499328123));
#36415=CARTESIAN_POINT('Ctrl Pts',(-8.29370291100539,-8.91422491072157,
-0.522917342403738));
#36416=CARTESIAN_POINT('Ctrl Pts',(-8.28671095382549,-8.89129327218942,
-0.783236938427221));
#36417=CARTESIAN_POINT('Ctrl Pts',(-8.24756465565675,-8.76290450544219,
-2.24070417726982));
#36418=CARTESIAN_POINT('Ctrl Pts',(-8.208418357488,-8.26862355942686,-3.66593985411726));
#36419=CARTESIAN_POINT('Ctrl Pts',(-8.16927205931926,-7.46706010555778,
-4.88994575979847));
#36420=CARTESIAN_POINT('Ctrl Pts',(-8.13012576115051,-6.6654966516887,-6.11395166547967));
#36421=CARTESIAN_POINT('Ctrl Pts',(-8.09097946298177,-5.55665068996587,
-7.13672779999466));
#36422=CARTESIAN_POINT('Ctrl Pts',(-8.05183316481303,-4.27200432179028,
-7.83699784537442));
#36423=CARTESIAN_POINT('Ctrl Pts',(-8.01268686664428,-2.9873579536147,-8.53726789075417));
#36424=CARTESIAN_POINT('Ctrl Pts',(-7.97354056847554,-1.52691117898638,
-8.91503184699869));
#36425=CARTESIAN_POINT('Ctrl Pts',(-7.93439427030679,-0.0638373849598622,
-8.92549611741949));
#36426=CARTESIAN_POINT('Ctrl Pts',(-7.89524797213805,1.39923640906668,-8.93596038784028));
#36427=CARTESIAN_POINT('Ctrl Pts',(-7.8561016739693,2.8649372224914,-8.57912497243734));
#36428=CARTESIAN_POINT('Ctrl Pts',(-7.81695537580056,4.15946866733332,-7.89730185311831));
#36429=CARTESIAN_POINT('Ctrl Pts',(-7.77780907763181,5.45400011217522,-7.21547873379928));
#36430=CARTESIAN_POINT('Ctrl Pts',(-7.73866277946307,6.5773621884343,-6.20866791056417));
#36431=CARTESIAN_POINT('Ctrl Pts',(-7.69951648129433,7.39635153737553,-4.99625260463822));
#36432=CARTESIAN_POINT('Ctrl Pts',(-7.66037018312558,8.21534088631675,-3.78383729871229));
#36433=CARTESIAN_POINT('Ctrl Pts',(-7.62122388495684,8.72995750794012,-2.3658175100955));
#36434=CARTESIAN_POINT('Ctrl Pts',(-7.5820775867881,8.87918041541532,-0.910335819517742));
#36435=CARTESIAN_POINT('Ctrl Pts',(-7.54293128861935,9.02840332289053,0.545145871060029));
#36436=CARTESIAN_POINT('Ctrl Pts',(-7.50378499045061,8.81223251621757,2.0380894635988));
#36437=CARTESIAN_POINT('Ctrl Pts',(-7.46463869228187,8.25630058360449,3.39146824059498));
#36438=CARTESIAN_POINT('Ctrl Pts',(-7.42549239411312,7.70036865099141,4.74484701759115));
#36439=CARTESIAN_POINT('Ctrl Pts',(-7.38634609594437,6.80467559243821,5.95866097904473));
#36440=CARTESIAN_POINT('Ctrl Pts',(-7.34719979777563,5.67542877092818,6.88898137752691));
#36441=CARTESIAN_POINT('Ctrl Pts',(-7.30805349960688,4.54618194941816,7.81930177600908));
#36442=CARTESIAN_POINT('Ctrl Pts',(-7.26890720143814,3.18338136495132,8.46612861151986));
#36443=CARTESIAN_POINT('Ctrl Pts',(-7.2297609032694,1.74862194669022,8.75276398866926));
#36444=CARTESIAN_POINT('Ctrl Pts',(-7.19061460510065,0.313862528429119,
9.03939936581866));
#36445=CARTESIAN_POINT('Ctrl Pts',(-7.15146830693191,-1.19285572362624,
8.96584328460668));
#36446=CARTESIAN_POINT('Ctrl Pts',(-7.11232200876316,-2.59287275313015,
8.54081770323353));
#36447=CARTESIAN_POINT('Ctrl Pts',(-7.07317571059442,-3.99288978263407,
8.11579212186038));
#36448=CARTESIAN_POINT('Ctrl Pts',(-7.03402941242568,-5.28620558958652,
7.33929704032606));
#36449=CARTESIAN_POINT('Ctrl Pts',(-6.99488311425694,-6.31946444565028,
6.30340584715549));
#36450=CARTESIAN_POINT('Ctrl Pts',(-6.95573681608819,-7.35272330171405,
5.26751465398492));
#36451=CARTESIAN_POINT('Ctrl Pts',(-6.91659051791944,-8.12592520688912,
3.97222734917811));
#36452=CARTESIAN_POINT('Ctrl Pts',(-6.8774442197507,-8.54738726309104,2.5711334326598));
#36453=CARTESIAN_POINT('Ctrl Pts',(-6.85419175495553,-8.79773102694041,
1.73889926256976));
#36454=CARTESIAN_POINT('Ctrl Pts',(-6.83093929016037,-8.92397296685791,
0.869334111825168));
#36455=CARTESIAN_POINT('Ctrl Pts',(-6.8076868253652,-8.92438047038815,-0.000115204162070208));
#36456=CARTESIAN_POINT('Origin',(-6.5,0.,0.));
#36457=CARTESIAN_POINT('',(-5.0923131746348,-8.92436978820107,0.000109438495129732));
#36458=CARTESIAN_POINT('',(-5.30768682536521,-8.92447940011954,0.000154963622128282));
#36459=CARTESIAN_POINT('',(-6.5,-8.925,-1.09299726823901E-15));
#36460=CARTESIAN_POINT('Ctrl Pts',(-5.0923131746348,-8.92436978820107,0.000109438495129732));
#36461=CARTESIAN_POINT('Ctrl Pts',(-5.1084106929876,-8.92463735146639,0.602025179022216));
#36462=CARTESIAN_POINT('Ctrl Pts',(-5.12450821134041,-8.86460350787768,
1.20388826880243));
#36463=CARTESIAN_POINT('Ctrl Pts',(-5.14060572969321,-8.74372518911622,
1.79327261198914));
#36464=CARTESIAN_POINT('Ctrl Pts',(-5.17975202786195,-8.44977064254175,
3.22655038367492));
#36465=CARTESIAN_POINT('Ctrl Pts',(-5.21889832603069,-7.79599659992567,
4.58603186904615));
#36466=CARTESIAN_POINT('Ctrl Pts',(-5.25804462419943,-6.85992472607204,
5.7105157031853));
#36467=CARTESIAN_POINT('Ctrl Pts',(-5.29719092236818,-5.92385285221839,
6.83499953732447));
#36468=CARTESIAN_POINT('Ctrl Pts',(-5.33633722053693,-4.70548314712719,
7.72448572023157));
#36469=CARTESIAN_POINT('Ctrl Pts',(-5.37548351870567,-3.34928455837054,
8.27350287307374));
#36470=CARTESIAN_POINT('Ctrl Pts',(-5.41462981687442,-1.99308596961389,
8.82252002591591));
#36471=CARTESIAN_POINT('Ctrl Pts',(-5.45377611504316,-0.499058497191769,
9.03106814869316));
#36472=CARTESIAN_POINT('Ctrl Pts',(-5.4929224132119,0.955642619659421,8.87441851769396));
#36473=CARTESIAN_POINT('Ctrl Pts',(-5.53206871138064,2.41034373651061,8.71776888669477));
#36474=CARTESIAN_POINT('Ctrl Pts',(-5.57121500954939,3.82571849779088,8.19592150191912));
#36475=CARTESIAN_POINT('Ctrl Pts',(-5.61036130771813,5.03393795853599,7.37075474244733));
#36476=CARTESIAN_POINT('Ctrl Pts',(-5.64950760588688,6.24215741928109,6.54558798297554));
#36477=CARTESIAN_POINT('Ctrl Pts',(-5.68865390405562,7.24322157949105,5.4171018488076));
#36478=CARTESIAN_POINT('Ctrl Pts',(-5.72780020222436,7.91842863209293,4.11910728704047));
#36479=CARTESIAN_POINT('Ctrl Pts',(-5.76694650039311,8.5936356846948,2.82111272527336));
#36480=CARTESIAN_POINT('Ctrl Pts',(-5.80609279856185,8.94298562968861,1.3536097359071));
#36481=CARTESIAN_POINT('Ctrl Pts',(-5.8452390967306,8.92505407948771,-0.109391598941135));
#36482=CARTESIAN_POINT('Ctrl Pts',(-5.88438539489934,8.90712252928682,-1.57239293378936));
#36483=CARTESIAN_POINT('Ctrl Pts',(-5.92353169306809,8.52190948389122,-3.03089261411952));
#36484=CARTESIAN_POINT('Ctrl Pts',(-5.96267799123683,7.81509182038236,-4.31194813079793));
#36485=CARTESIAN_POINT('Ctrl Pts',(-6.00182428940557,7.10827415687349,-5.59300364747637));
#36486=CARTESIAN_POINT('Ctrl Pts',(-6.04097058757431,6.07985187525134,-6.69661500050304));
#36487=CARTESIAN_POINT('Ctrl Pts',(-6.08011688574306,4.85177078889619,-7.49192078546702));
#36488=CARTESIAN_POINT('Ctrl Pts',(-6.11926318391181,3.62368970254106,-8.28722657043099));
#36489=CARTESIAN_POINT('Ctrl Pts',(-6.15840948208055,2.19594981145294,-8.77422678733228));
#36490=CARTESIAN_POINT('Ctrl Pts',(-6.1975557802493,0.737846263573978,-8.89517508175242));
#36491=CARTESIAN_POINT('Ctrl Pts',(-6.23670207841804,-0.720257284304982,
-9.01612337617255));
#36492=CARTESIAN_POINT('Ctrl Pts',(-6.27584837658678,-2.20872448897478,
-8.77101974811154));
#36493=CARTESIAN_POINT('Ctrl Pts',(-6.31499467475553,-3.55105942341503,
-8.18892751311638));
#36494=CARTESIAN_POINT('Ctrl Pts',(-6.35414097292427,-4.89339435785525,
-7.60683527812123));
#36495=CARTESIAN_POINT('Ctrl Pts',(-6.39328727109301,-6.08959702206593,
-6.68775443619196));
#36496=CARTESIAN_POINT('Ctrl Pts',(-6.43243356926176,-6.9978269391714,-5.54066557131056));
#36497=CARTESIAN_POINT('Ctrl Pts',(-6.4715798674305,-7.90605685627687,-4.39357670642917));
#36498=CARTESIAN_POINT('Ctrl Pts',(-6.51072616559924,-8.52631402627713,
-3.01847981859566));
#36499=CARTESIAN_POINT('Ctrl Pts',(-6.54987246376799,-8.78505106843932,
-1.57842787881243));
#36500=CARTESIAN_POINT('Ctrl Pts',(-6.56401936739026,-8.87855487774464,
-1.05801402217245));
#36501=CARTESIAN_POINT('Ctrl Pts',(-6.57816627101252,-8.92484435259045,
-0.529117070646644));
#36502=CARTESIAN_POINT('Ctrl Pts',(-6.59231317463479,-8.9244947065883,-0.000159621216041517));
#36503=CARTESIAN_POINT('Ctrl Pts',(-6.8076868253652,-8.92438047038815,-0.000115204162070208));
#36504=CARTESIAN_POINT('Ctrl Pts',(-6.79179299199162,-8.92465901261006,
-0.594412741081523));
#36505=CARTESIAN_POINT('Ctrl Pts',(-6.77589915861805,-8.86614547439013,
-1.18865615794793));
#36506=CARTESIAN_POINT('Ctrl Pts',(-6.76000532524447,-8.74828653057556,
-1.77088648217279));
#36507=CARTESIAN_POINT('Ctrl Pts',(-6.72085902707572,-8.45800153462939,
-3.20491195225729));
#36508=CARTESIAN_POINT('Ctrl Pts',(-6.68171272890698,-7.80770933550826,
-4.5660623641965));
#36509=CARTESIAN_POINT('Ctrl Pts',(-6.64256643073823,-6.87451873625329,
-5.69293845906439));
#36510=CARTESIAN_POINT('Ctrl Pts',(-6.60342013256949,-5.94132813699833,
-6.81981455393227));
#36511=CARTESIAN_POINT('Ctrl Pts',(-6.56427383440075,-4.72523913760954,
-7.71241633172884));
#36512=CARTESIAN_POINT('Ctrl Pts',(-6.52512753623201,-3.37045024955766,
-8.26490298001428));
#36513=CARTESIAN_POINT('Ctrl Pts',(-6.48598123806326,-2.01566136150579,
-8.81738962829971));
#36514=CARTESIAN_POINT('Ctrl Pts',(-6.44683493989451,-0.522172584790831,
-9.02976114707401));
#36515=CARTESIAN_POINT('Ctrl Pts',(-6.40768864172577,0.932924717530035,
-8.87683545106101));
#36516=CARTESIAN_POINT('Ctrl Pts',(-6.36854234355703,2.38802201985091,-8.72390975504801));
#36517=CARTESIAN_POINT('Ctrl Pts',(-6.32939604538828,3.80472784777769,-8.20568684424769));
#36518=CARTESIAN_POINT('Ctrl Pts',(-6.29024974721954,5.01505542428857,-7.38361532347845));
#36519=CARTESIAN_POINT('Ctrl Pts',(-6.2511034490508,6.22538300079946,-6.56154380270922));
#36520=CARTESIAN_POINT('Ctrl Pts',(-6.21195715088205,7.22933232589443,-5.43562367197108));
#36521=CARTESIAN_POINT('Ctrl Pts',(-6.17281085271331,7.90785948227508,-4.1393616129041));
#36522=CARTESIAN_POINT('Ctrl Pts',(-6.13366455454456,8.58638663865573,-2.84309955383713));
#36523=CARTESIAN_POINT('Ctrl Pts',(-6.09451825637582,8.93949162632205,-1.37649556644134));
#36524=CARTESIAN_POINT('Ctrl Pts',(-6.05537195820708,8.92530480116083,0.086546866885319));
#36525=CARTESIAN_POINT('Ctrl Pts',(-6.01622566003833,8.9111179759996,1.54958930021198));
#36526=CARTESIAN_POINT('Ctrl Pts',(-5.97707936186958,8.52963933801083,3.00907017946953));
#36527=CARTESIAN_POINT('Ctrl Pts',(-5.93793306370084,7.82610295458887,4.29193064924951));
#36528=CARTESIAN_POINT('Ctrl Pts',(-5.89878676553209,7.12256657116693,5.57479111902946));
#36529=CARTESIAN_POINT('Ctrl Pts',(-5.85964046736335,6.09697244231183,6.68103117933188));
#36530=CARTESIAN_POINT('Ctrl Pts',(-5.82049416919461,4.8709310314258,7.47947772514133));
#36531=CARTESIAN_POINT('Ctrl Pts',(-5.78134787102587,3.64488962053974,8.2779242709508));
#36532=CARTESIAN_POINT('Ctrl Pts',(-5.74220157285712,2.21840092762276,8.76857730226729));
#36533=CARTESIAN_POINT('Ctrl Pts',(-5.70305527468838,0.760611739013584,
8.89325732992511));
#36534=CARTESIAN_POINT('Ctrl Pts',(-5.66390897651963,-0.697177449595592,
9.01793735758293));
#36535=CARTESIAN_POINT('Ctrl Pts',(-5.62476267835089,-2.18626713389695,
8.77664438158209));
#36536=CARTESIAN_POINT('Ctrl Pts',(-5.58561638018215,-3.5300875759596,8.19798986702519));
#36537=CARTESIAN_POINT('Ctrl Pts',(-5.5464700820134,-4.87390801802225,7.61933535246829));
#36538=CARTESIAN_POINT('Ctrl Pts',(-5.50732378384466,-6.07245921784618,
6.70331929935531));
#36539=CARTESIAN_POINT('Ctrl Pts',(-5.46817748567591,-6.98362221948084,
5.55855888242316));
#36540=CARTESIAN_POINT('Ctrl Pts',(-5.42903118750717,-7.8947852211155,4.41379846549101));
#36541=CARTESIAN_POINT('Ctrl Pts',(-5.38988488933843,-8.51856002456089,
3.04029368473968));
#36542=CARTESIAN_POINT('Ctrl Pts',(-5.35073859116968,-8.7809821435047,1.60090872608144));
#36543=CARTESIAN_POINT('Ctrl Pts',(-5.33638800256819,-8.87718311384068,
1.07324653713474));
#36544=CARTESIAN_POINT('Ctrl Pts',(-5.3220374139667,-8.92482289482857,0.536730893015737));
#36545=CARTESIAN_POINT('Ctrl Pts',(-5.30768682536521,-8.92447940011954,
0.000154963622128282));
#36546=CARTESIAN_POINT('Origin',(-6.5,0.,0.));
#36547=CARTESIAN_POINT('',(-3.59231317463479,-8.92520804921716,0.00020252989606076));
#36548=CARTESIAN_POINT('',(-3.80768682536521,-8.9253958274169,0.000172963988443203));
#36549=CARTESIAN_POINT('',(-6.5,-8.925,-1.09299726823901E-15));
#36550=CARTESIAN_POINT('Ctrl Pts',(-3.59231317463479,-8.92520804921716,
0.00020252989606076));
#36551=CARTESIAN_POINT('Ctrl Pts',(-3.59950881679392,-8.92547024676361,
0.269188130100031));
#36552=CARTESIAN_POINT('Ctrl Pts',(-3.60670445895305,-8.9135447392344,0.538150566983954));
#36553=CARTESIAN_POINT('Ctrl Pts',(-3.61390010111218,-8.88925943030047,
0.805992336250304));
#36554=CARTESIAN_POINT('Ctrl Pts',(-3.65304639928093,-8.75714058341735,
2.26312618613775));
#36555=CARTESIAN_POINT('Ctrl Pts',(-3.69219269744967,-8.25921324989963,
3.68709204960042));
#36556=CARTESIAN_POINT('Ctrl Pts',(-3.73133899561841,-7.45451947889753,
4.90904228672834));
#36557=CARTESIAN_POINT('Ctrl Pts',(-3.77048529378716,-6.64982570789543,
6.13099252385626));
#36558=CARTESIAN_POINT('Ctrl Pts',(-3.8096315919559,-5.53836549940895,7.15092713464943));
#36559=CARTESIAN_POINT('Ctrl Pts',(-3.84877789012465,-4.25193093820849,
7.84790673640995));
#36560=CARTESIAN_POINT('Ctrl Pts',(-3.88792418829339,-2.96549637700803,
8.54488633817046));
#36561=CARTESIAN_POINT('Ctrl Pts',(-3.92707048646213,-1.5040874630936,8.91891093089831));
#36562=CARTESIAN_POINT('Ctrl Pts',(-3.96621678463088,-0.0409916710908219,
8.92563031535538));
#36563=CARTESIAN_POINT('Ctrl Pts',(-4.00536308279962,1.42210412091196,8.93234969981245));
#36564=CARTESIAN_POINT('Ctrl Pts',(-4.04450938096837,2.88688679100308,8.57176387599873));
#36565=CARTESIAN_POINT('Ctrl Pts',(-4.08365567913711,4.17966882128255,7.88662953279256));
#36566=CARTESIAN_POINT('Ctrl Pts',(-4.12280197730586,5.472450851562,7.20149518958641));
#36567=CARTESIAN_POINT('Ctrl Pts',(-4.1619482754746,6.59323224202979,6.19181232698781));
#36568=CARTESIAN_POINT('Ctrl Pts',(-4.20109457364334,7.40911564004151,4.97730472010364));
#36569=CARTESIAN_POINT('Ctrl Pts',(-4.24024087181208,8.22499903805323,3.76279711321948));
#36570=CARTESIAN_POINT('Ctrl Pts',(-4.27938716998083,8.73598444360888,2.34346476204975));
#36571=CARTESIAN_POINT('Ctrl Pts',(-4.31853346814957,8.88148144375866,0.887605885235826));
#36572=CARTESIAN_POINT('Ctrl Pts',(-4.35767976631832,9.02697844390845,-0.568252991578145));
#36573=CARTESIAN_POINT('Ctrl Pts',(-4.39682606448706,8.80698703865234,-2.06063839403631));
#36574=CARTESIAN_POINT('Ctrl Pts',(-4.43597236265581,8.24759284597125,-3.41258979236604));
#36575=CARTESIAN_POINT('Ctrl Pts',(-4.47511866082455,7.68819865329017,-4.76454119069574));
#36576=CARTESIAN_POINT('Ctrl Pts',(-4.5142649589933,6.78940167318409,-5.97605858489704));
#36577=CARTESIAN_POINT('Ctrl Pts',(-4.55341125716204,5.65777731811414,-6.90348554443819));
#36578=CARTESIAN_POINT('Ctrl Pts',(-4.59255755533079,4.52615296304418,-7.83091250397935));
#36579=CARTESIAN_POINT('Ctrl Pts',(-4.63170385349953,3.16170123301033,-8.47424902886039));
#36580=CARTESIAN_POINT('Ctrl Pts',(-4.67085015166827,1.72621284276808,-8.75721108944933));
#36581=CARTESIAN_POINT('Ctrl Pts',(-4.70999644983701,0.290724452525837,
-9.04017315003826));
#36582=CARTESIAN_POINT('Ctrl Pts',(-4.74914274800576,-1.2158005979248,-8.9627607463351));
#36583=CARTESIAN_POINT('Ctrl Pts',(-4.7882890461745,-2.61472516122752,-8.53415310238505));
#36584=CARTESIAN_POINT('Ctrl Pts',(-4.82743534434325,-4.01364972453022,
-8.10554545843501));
#36585=CARTESIAN_POINT('Ctrl Pts',(-4.86658164251199,-5.30497380068501,
-7.3257425742381));
#36586=CARTESIAN_POINT('Ctrl Pts',(-4.90572794068074,-6.33557783208182,
-6.28721006308237));
#36587=CARTESIAN_POINT('Ctrl Pts',(-4.94487423884948,-7.36618186347866,
-5.24867755192661));
#36588=CARTESIAN_POINT('Ctrl Pts',(-4.98402053701822,-8.13606585011751,
-3.95141541381203));
#36589=CARTESIAN_POINT('Ctrl Pts',(-5.02316683518697,-8.55394031817052,
-2.54924731575455));
#36590=CARTESIAN_POINT('Ctrl Pts',(-5.04621561500291,-8.79997882130919,
-1.72367081762046));
#36591=CARTESIAN_POINT('Ctrl Pts',(-5.06926439481886,-8.92398668524979,
-0.861726719544906));
#36592=CARTESIAN_POINT('Ctrl Pts',(-5.0923131746348,-8.92436978820107,0.000109438495129732));
#36593=CARTESIAN_POINT('Ctrl Pts',(-5.30768682536521,-8.92447940011954,
0.000154963622128282));
#36594=CARTESIAN_POINT('Ctrl Pts',(-5.28289111579795,-8.92388589170818,
-0.926969440504354));
#36595=CARTESIAN_POINT('Ctrl Pts',(-5.2580954062307,-8.78003944268694,-1.85427382489975));
#36596=CARTESIAN_POINT('Ctrl Pts',(-5.23329969666344,-8.49592120033681,
-2.73639893134377));
#36597=CARTESIAN_POINT('Ctrl Pts',(-5.1941533984947,-8.04736870378287,-4.12905649354552));
#36598=CARTESIAN_POINT('Ctrl Pts',(-5.15500710032596,-7.24919427623276,
-5.40910648138388));
#36599=CARTESIAN_POINT('Ctrl Pts',(-5.11586080215721,-6.19604194818467,
-6.42476616929583));
#36600=CARTESIAN_POINT('Ctrl Pts',(-5.07671450398847,-5.14288962013658,
-7.44042585720777));
#36601=CARTESIAN_POINT('Ctrl Pts',(-5.03756820581973,-3.83475939159051,
-8.19169524519331));
#36602=CARTESIAN_POINT('Ctrl Pts',(-4.99842190765098,-2.42676362016271,
-8.58949209707109));
#36603=CARTESIAN_POINT('Ctrl Pts',(-4.95927560948224,-1.0187678487349,-8.98728894894888));
#36604=CARTESIAN_POINT('Ctrl Pts',(-4.92012931131349,0.489093465574642,
-9.0316132647189));
#36605=CARTESIAN_POINT('Ctrl Pts',(-4.88098301314475,1.91802472710077,-8.71720926099757));
#36606=CARTESIAN_POINT('Ctrl Pts',(-4.84183671497601,3.34695598862691,-8.40280525727623));
#36607=CARTESIAN_POINT('Ctrl Pts',(-4.80269041680727,4.69695719736963,-7.72967293406355));
#36608=CARTESIAN_POINT('Ctrl Pts',(-4.76354411863852,5.80795111812432,-6.77762937635807));
#36609=CARTESIAN_POINT('Ctrl Pts',(-4.72439782046978,6.91894503887903,-5.82558581865258));
#36610=CARTESIAN_POINT('Ctrl Pts',(-4.68525152230103,7.7909316716457,-4.59463102645427));
#36611=CARTESIAN_POINT('Ctrl Pts',(-4.64610522413228,8.32051465766307,-3.230726231887));
#36612=CARTESIAN_POINT('Ctrl Pts',(-4.60695892596354,8.85009764368042,-1.86682143731975));
#36613=CARTESIAN_POINT('Ctrl Pts',(-4.5678126277948,9.03727698294849,-0.369966640383566));
#36614=CARTESIAN_POINT('Ctrl Pts',(-4.52866632962606,8.85985776858471,1.08234766791798));
#36615=CARTESIAN_POINT('Ctrl Pts',(-4.48952003145731,8.68243855422092,2.53466197621952));
#36616=CARTESIAN_POINT('Ctrl Pts',(-4.45037373328856,8.14042078622527,3.9424357958864));
#36617=CARTESIAN_POINT('Ctrl Pts',(-4.41122743511982,7.29807455944982,5.13874146834563));
#36618=CARTESIAN_POINT('Ctrl Pts',(-4.37208113695108,6.45572833267433,6.33504714080488));
#36619=CARTESIAN_POINT('Ctrl Pts',(-4.33293483878233,5.31305364711901,7.31988466605648));
#36620=CARTESIAN_POINT('Ctrl Pts',(-4.29378854061359,4.005543866204,7.97647632038817));
#36621=CARTESIAN_POINT('Ctrl Pts',(-4.25464224244485,2.69803408528902,8.63306797471983));
#36622=CARTESIAN_POINT('Ctrl Pts',(-4.2154959442761,1.22568920901436,8.96141375813161));
#36623=CARTESIAN_POINT('Ctrl Pts',(-4.17634964610736,-0.236906550731843,
8.92257986459216));
#36624=CARTESIAN_POINT('Ctrl Pts',(-4.13720334793861,-1.69950231047808,
8.88374597105271));
#36625=CARTESIAN_POINT('Ctrl Pts',(-4.09805704976987,-3.15234895369587,
8.47773240056201));
#36626=CARTESIAN_POINT('Ctrl Pts',(-4.05891075160112,-4.42317428367459,
7.75268246544155));
#36627=CARTESIAN_POINT('Ctrl Pts',(-4.01976445343238,-5.69399961365327,
7.02763253032112));
#36628=CARTESIAN_POINT('Ctrl Pts',(-3.98061815526363,-6.7828036303929,5.98354623057094));
#36629=CARTESIAN_POINT('Ctrl Pts',(-3.94147185709489,-7.56048071857314,
4.74422675027843));
#36630=CARTESIAN_POINT('Ctrl Pts',(-3.90232555892615,-8.33815780675341,
3.50490726998588));
#36631=CARTESIAN_POINT('Ctrl Pts',(-3.8631792607574,-8.80470796637427,2.07035460915098));
#36632=CARTESIAN_POINT('Ctrl Pts',(-3.82403296258866,-8.90480972139819,
0.610671744158159));
#36633=CARTESIAN_POINT('Ctrl Pts',(-3.81858425018084,-8.91874272911943,
0.407500754562134));
#36634=CARTESIAN_POINT('Ctrl Pts',(-3.81313553777302,-8.92557637671001,
0.203842906878487));
#36635=CARTESIAN_POINT('Ctrl Pts',(-3.80768682536521,-8.9253958274169,0.000172963988443203));
#36636=CARTESIAN_POINT('Origin',(-6.5,0.,0.));
#36637=CARTESIAN_POINT('',(-2.09231317463479,-8.92567592894044,-6.35753767513903E-5));
#36638=CARTESIAN_POINT('',(-2.3076868253652,-8.92557695889132,-0.000120900814251108));
#36639=CARTESIAN_POINT('',(-6.5,-8.925,-1.09299726823901E-15));
#36640=CARTESIAN_POINT('Ctrl Pts',(-2.09231317463479,-8.92567592894044,
-6.35753767513903E-5));
#36641=CARTESIAN_POINT('Ctrl Pts',(-2.12975323876899,-8.92512744453285,
1.39929403128198));
#36642=CARTESIAN_POINT('Ctrl Pts',(-2.16719330290319,-8.59027658419489,
2.79890392264426));
#36643=CARTESIAN_POINT('Ctrl Pts',(-2.20463336703739,-7.95593258617703,
4.04620331871739));
#36644=CARTESIAN_POINT('Ctrl Pts',(-2.24377966520614,-7.29268000202141,
5.35034515697271));
#36645=CARTESIAN_POINT('Ctrl Pts',(-2.28292596337488,-6.30201503000759,
6.48797786134668));
#36646=CARTESIAN_POINT('Ctrl Pts',(-2.32207226154363,-5.10142365877174,
7.32420712829358));
#36647=CARTESIAN_POINT('Ctrl Pts',(-2.36121855971237,-3.9008322875359,8.16043639524047));
#36648=CARTESIAN_POINT('Ctrl Pts',(-2.40036485788111,-2.49031451707803,
8.69526222476028));
#36649=CARTESIAN_POINT('Ctrl Pts',(-2.43951115604986,-1.0371146030729,8.86526669949332));
#36650=CARTESIAN_POINT('Ctrl Pts',(-2.4786574542186,0.416085310932213,9.03527117422634));
#36651=CARTESIAN_POINT('Ctrl Pts',(-2.51780375238735,1.91196736848452,8.84045429417261));
#36652=CARTESIAN_POINT('Ctrl Pts',(-2.55695005055609,3.27315197002397,8.30391690262062));
#36653=CARTESIAN_POINT('Ctrl Pts',(-2.59609634872483,4.63433657156346,7.76737951106861));
#36654=CARTESIAN_POINT('Ctrl Pts',(-2.63524264689358,5.86082371709005,6.88912160801828));
#36655=CARTESIAN_POINT('Ctrl Pts',(-2.67438894506232,6.80718418858864,5.77328301450695));
#36656=CARTESIAN_POINT('Ctrl Pts',(-2.71353524323107,7.7535446600872,4.65744442099566));
#36657=CARTESIAN_POINT('Ctrl Pts',(-2.75268154139981,8.41977845755782,3.30402513702336));
#36658=CARTESIAN_POINT('Ctrl Pts',(-2.79182783956856,8.7268853455449,1.87350777816278));
#36659=CARTESIAN_POINT('Ctrl Pts',(-2.8309741377373,9.03399223353197,0.442990419302195));
#36660=CARTESIAN_POINT('Ctrl Pts',(-2.87012043590604,8.9819722120355,-1.06462501444667));
#36661=CARTESIAN_POINT('Ctrl Pts',(-2.90926673407479,8.57699417009785,-2.47057212345786));
#36662=CARTESIAN_POINT('Ctrl Pts',(-2.94841303224353,8.17201612816018,-3.87651923246909));
#36663=CARTESIAN_POINT('Ctrl Pts',(-2.98755933041227,7.41408006578131,-5.18079801674265));
#36664=CARTESIAN_POINT('Ctrl Pts',(-3.02670562858102,6.39305842845737,-6.22875278545715));
#36665=CARTESIAN_POINT('Ctrl Pts',(-3.06585192674976,5.37203679113344,-7.27670755417164));
#36666=CARTESIAN_POINT('Ctrl Pts',(-3.10499822491851,4.08792957886444,-8.06833830732709));
#36667=CARTESIAN_POINT('Ctrl Pts',(-3.14414452308726,2.69300075528545,-8.50977694516169));
#36668=CARTESIAN_POINT('Ctrl Pts',(-3.183290821256,1.29807193170646,-8.95121558299629));
#36669=CARTESIAN_POINT('Ctrl Pts',(-3.22243711942474,-0.207678503182533,
-9.04246210551005));
#36670=CARTESIAN_POINT('Ctrl Pts',(-3.26158341759348,-1.64570532879268,
-8.77269689408073));
#36671=CARTESIAN_POINT('Ctrl Pts',(-3.30072971576223,-3.08373215440282,
-8.50293168265141));
#36672=CARTESIAN_POINT('Ctrl Pts',(-3.33987601393097,-4.45403537073412,
-7.87215473727899));
#36673=CARTESIAN_POINT('Ctrl Pts',(-3.37902231209972,-5.59413038066898,
-6.95516083031861));
#36674=CARTESIAN_POINT('Ctrl Pts',(-3.41816861026846,-6.73422539060384,
-6.03816692335823));
#36675=CARTESIAN_POINT('Ctrl Pts',(-3.45731490843721,-7.64411219414225,
-4.83495605480989));
#36676=CARTESIAN_POINT('Ctrl Pts',(-3.49646120660595,-8.21590041578719,
-3.4881997023796));
#36677=CARTESIAN_POINT('Ctrl Pts',(-3.52841186261556,-8.68258589141955,
-2.38899617718856));
#36678=CARTESIAN_POINT('Ctrl Pts',(-3.56036251862518,-8.92404381905845,
-1.19416847877798));
#36679=CARTESIAN_POINT('Ctrl Pts',(-3.59231317463479,-8.92520804921716,
0.00020252989606076));
#36680=CARTESIAN_POINT('Ctrl Pts',(-3.80768682536521,-8.9253958274169,0.000172963988443203));
#36681=CARTESIAN_POINT('Ctrl Pts',(-3.77398923960428,-8.92427921952252,
-1.25942469024143));
#36682=CARTESIAN_POINT('Ctrl Pts',(-3.74029165384335,-8.65488294674644,
-2.51948496306796));
#36683=CARTESIAN_POINT('Ctrl Pts',(-3.70659406808243,-8.13735199258016,
-3.66770482771282));
#36684=CARTESIAN_POINT('Ctrl Pts',(-3.66744776991368,-7.53613915831117,
-5.00158546544041));
#36685=CARTESIAN_POINT('Ctrl Pts',(-3.62830147174494,-6.60006013934619,
-6.18453367174483));
#36686=CARTESIAN_POINT('Ctrl Pts',(-3.58915517357619,-5.44011108944268,
-7.07628062528088));
#36687=CARTESIAN_POINT('Ctrl Pts',(-3.55000887540745,-4.28016203953921,
-7.9680275788169));
#36688=CARTESIAN_POINT('Ctrl Pts',(-3.51086257723871,-2.89634295869721,
-8.56857327958457));
#36689=CARTESIAN_POINT('Ctrl Pts',(-3.47171627906996,-1.45274105673856,
-8.80670764676786));
#36690=CARTESIAN_POINT('Ctrl Pts',(-3.43256998090122,-0.00913915477988414,
-9.04484201395115));
#36691=CARTESIAN_POINT('Ctrl Pts',(-3.39342368273248,1.49424556829545,-8.92056504755005));
#36692=CARTESIAN_POINT('Ctrl Pts',(-3.35427738456373,2.87914833012853,-8.44861296604076));
#36693=CARTESIAN_POINT('Ctrl Pts',(-3.31513108639499,4.26405109196163,-7.97666088453146));
#36694=CARTESIAN_POINT('Ctrl Pts',(-3.27598478822624,5.53047189255247,-7.15703368791396));
#36695=CARTESIAN_POINT('Ctrl Pts',(-3.23683849005749,6.52824409825605,-6.08691918277787));
#36696=CARTESIAN_POINT('Ctrl Pts',(-3.19769219188875,7.52601630395961,-5.01680467764181));
#36697=CARTESIAN_POINT('Ctrl Pts',(-3.15854589372001,8.25513991477593,-3.69620286398717));
#36698=CARTESIAN_POINT('Ctrl Pts',(-3.11939959555127,8.62915863886055,-2.2817049241895));
#36699=CARTESIAN_POINT('Ctrl Pts',(-3.08025329738252,9.00317736294517,-0.86720698439182));
#36700=CARTESIAN_POINT('Ctrl Pts',(-3.04110699921378,9.02209120029809,0.641187081548901));
#36701=CARTESIAN_POINT('Ctrl Pts',(-3.00196070104503,8.68365744070487,2.06461850420449));
#36702=CARTESIAN_POINT('Ctrl Pts',(-2.96281440287629,8.34522368111165,3.4880499268601));
#36703=CARTESIAN_POINT('Ctrl Pts',(-2.92366810470755,7.64944232457228,4.82651870623058));
#36704=CARTESIAN_POINT('Ctrl Pts',(-2.8845218065388,6.67881605995841,5.92131507685209));
#36705=CARTESIAN_POINT('Ctrl Pts',(-2.84537550837006,5.70818979534454,7.01611144747359));
#36706=CARTESIAN_POINT('Ctrl Pts',(-2.80622921020131,4.46271862265616,7.86723540934612));
#36707=CARTESIAN_POINT('Ctrl Pts',(-2.76708291203257,3.09008510102932,8.37376439859726));
#36708=CARTESIAN_POINT('Ctrl Pts',(-2.72793661386383,1.71745157940249,8.88029338784841));
#36709=CARTESIAN_POINT('Ctrl Pts',(-2.68879031569508,0.217655708837203,
9.04222740447817));
#36710=CARTESIAN_POINT('Ctrl Pts',(-2.64964401752634,-1.23146335510331,
8.84036503982962));
#36711=CARTESIAN_POINT('Ctrl Pts',(-2.61049771935759,-2.68058241904383,
8.63850267518107));
#36712=CARTESIAN_POINT('Ctrl Pts',(-2.57135142118885,-4.07902467635957,
8.07284392925421));
#36713=CARTESIAN_POINT('Ctrl Pts',(-2.5322051230201,-5.26096881651629,7.21046210448127));
#36714=CARTESIAN_POINT('Ctrl Pts',(-2.49305882485136,-6.442912956673,6.34808027970835));
#36715=CARTESIAN_POINT('Ctrl Pts',(-2.45391252668262,-7.40835897967068,
5.18897537608936));
#36716=CARTESIAN_POINT('Ctrl Pts',(-2.41476622851387,-8.04282881216971,
3.87058905149697));
#36717=CARTESIAN_POINT('Ctrl Pts',(-2.37907309413098,-8.62133094526183,
2.66849990249503));
#36718=CARTESIAN_POINT('Ctrl Pts',(-2.34337995974809,-8.92467344142811,
1.33399090208915));
#36719=CARTESIAN_POINT('Ctrl Pts',(-2.3076868253652,-8.92557695889132,-0.000120900814251108));
#36720=CARTESIAN_POINT('Origin',(-14.3478126690739,0.,0.));
#36721=CARTESIAN_POINT('',(-1.59781266907387,-8.06911106248246,-5.74742776433716E-5));
#36722=CARTESIAN_POINT('',(-1.5,-8.0685,-1.61713948722842E-13));
#36723=CARTESIAN_POINT('',(-14.3478126690739,-8.0685,-1.61713948722842E-13));
#36724=CARTESIAN_POINT('',(-1.5,-7.40070004445565,-3.21408324440955));
#36725=CARTESIAN_POINT('Ctrl Pts',(-1.59781266907387,-8.06911106248246,
-5.74742776435905E-5));
#36726=CARTESIAN_POINT('Ctrl Pts',(-1.59610643503933,-8.06913365948742,
-0.0577095977506832));
#36727=CARTESIAN_POINT('Ctrl Pts',(-1.56350221201471,-8.05757148270878,
-1.15936810984891));
#36728=CARTESIAN_POINT('Ctrl Pts',(-1.53089798899008,-7.81573019911042,
-2.25608704898405));
#36729=CARTESIAN_POINT('Ctrl Pts',(-1.5,-7.40071554151276,-3.21429017473183));
#36730=CARTESIAN_POINT('Origin',(-1.5,0.,0.));
#36731=CARTESIAN_POINT('Origin',(-14.3478126690739,0.,0.));
#36732=CARTESIAN_POINT('',(-3.09781266907387,-8.06868808348557,0.000183093833578688));
#36733=CARTESIAN_POINT('',(-2.80218733092611,-8.06902159023133,-0.000109298400164937));
#36734=CARTESIAN_POINT('',(-14.3478126690739,-8.0685,-1.61713948722842E-13));
#36735=CARTESIAN_POINT('Ctrl Pts',(-3.09781266907387,-8.06868808348557,
0.000183093833578535));
#36736=CARTESIAN_POINT('Ctrl Pts',(-3.06586201306426,-8.06763558028828,
-1.07956844493236));
#36737=CARTESIAN_POINT('Ctrl Pts',(-2.9947650588859,-7.58190296737274,-3.48316225362576));
#36738=CARTESIAN_POINT('Ctrl Pts',(-2.8845218065388,-5.26539785879409,-6.54644893154043));
#36739=CARTESIAN_POINT('Ctrl Pts',(-2.76708291203257,-1.54899735426666,
-8.25717961514961));
#36740=CARTESIAN_POINT('Ctrl Pts',(-2.64964401752634,2.53474966553227,-8.00970984476226));
#36741=CARTESIAN_POINT('Ctrl Pts',(-2.5322051230201,6.01737791500869,-5.86272741389347));
#36742=CARTESIAN_POINT('Ctrl Pts',(-2.41476622851387,8.07297694670747,-2.3253918270326));
#36743=CARTESIAN_POINT('Ctrl Pts',(-2.29732733400764,8.21406049072235,1.76341325774147));
#36744=CARTESIAN_POINT('Ctrl Pts',(-2.17988843950141,6.4071672487419,5.43402283512993));
#36745=CARTESIAN_POINT('Ctrl Pts',(-2.06244954499518,3.08081043069796,7.81594683202442));
#36746=CARTESIAN_POINT('Ctrl Pts',(-1.94501065048894,-0.976172554633629,
8.34430985612986));
#36747=CARTESIAN_POINT('Ctrl Pts',(-1.82757175598271,-4.80163898520143,
6.89380827445569));
#36748=CARTESIAN_POINT('Ctrl Pts',(-1.71183909551102,-7.44938682960104,
3.85326013172529));
#36749=CARTESIAN_POINT('Ctrl Pts',(-1.63525273320807,-8.06861521414156,
1.26500883937235));
#36750=CARTESIAN_POINT('Ctrl Pts',(-1.59781266907387,-8.06911106248246,
-5.74742776435905E-5));
#36751=CARTESIAN_POINT('',(-1.5,-5.45359047959038,5.94634704090849));
#36752=CARTESIAN_POINT('Origin',(-1.5,0.,0.));
#36753=CARTESIAN_POINT('Ctrl Pts',(-2.80218733092611,-8.06902159023132,
-0.000109298400165197));
#36754=CARTESIAN_POINT('Ctrl Pts',(-2.79873416714026,-8.06910061325082,
-0.11679275755619));
#36755=CARTESIAN_POINT('Ctrl Pts',(-2.75613470518566,-8.03850549293377,
-1.55620012847858));
#36756=CARTESIAN_POINT('Ctrl Pts',(-2.67438894506232,-7.2259267400895,-4.28560128601273));
#36757=CARTESIAN_POINT('Ctrl Pts',(-2.55695005055609,-4.34491343911961,
-7.1904203216184));
#36758=CARTESIAN_POINT('Ctrl Pts',(-2.43951115604986,-0.433490517027392,
-8.39002416011216));
#36759=CARTESIAN_POINT('Ctrl Pts',(-2.32207226154363,3.58071951422406,-7.59991946597854));
#36760=CARTESIAN_POINT('Ctrl Pts',(-2.20463336703739,6.74578836548944,-5.00749194802054));
#36761=CARTESIAN_POINT('Ctrl Pts',(-2.08719447253116,8.31102423036551,-1.22751659427962));
#36762=CARTESIAN_POINT('Ctrl Pts',(-1.96975557802493,7.90541015591722,2.84353655923596));
#36763=CARTESIAN_POINT('Ctrl Pts',(-1.8523166835187,5.62478208560713,6.24029926664823));
#36764=CARTESIAN_POINT('Ctrl Pts',(-1.73487778901246,2.01069766784778,8.15705187872645));
#36765=CARTESIAN_POINT('Ctrl Pts',(-1.61743889450623,-2.08118048114745,
8.1395942446814));
#36766=CARTESIAN_POINT('Ctrl Pts',(-1.53914629816874,-4.4785344754388,6.8406029773222));
#36767=CARTESIAN_POINT('Ctrl Pts',(-1.5,-5.45359047959038,5.94634704090849));
#36768=CARTESIAN_POINT('Origin',(-14.3478126690739,0.,0.));
#36769=CARTESIAN_POINT('',(-4.59781266907387,-8.06793026735018,9.89360780153199E-5));
#36770=CARTESIAN_POINT('',(-4.30218733092611,-8.06885784129,0.000156365259223884));
#36771=CARTESIAN_POINT('',(-14.3478126690739,-8.0685,-1.61713948722842E-13));
#36772=CARTESIAN_POINT('Ctrl Pts',(-4.59781266907387,-8.06793026735018,
9.89360780155601E-5));
#36773=CARTESIAN_POINT('Ctrl Pts',(-4.57476388925793,-8.0675839294048,-0.779029920072743));
#36774=CARTESIAN_POINT('Ctrl Pts',(-4.51256881127325,-7.76507243369392,
-2.88170300903797));
#36775=CARTESIAN_POINT('Ctrl Pts',(-4.41122743511982,-5.96327500496155,
-5.91774951138349));
#36776=CARTESIAN_POINT('Ctrl Pts',(-4.29378854061358,-2.46107389287582,
-8.03265356891045));
#36777=CARTESIAN_POINT('Ctrl Pts',(-4.17634964610736,1.62477396243877,-8.24260381404624));
#36778=CARTESIAN_POINT('Ctrl Pts',(-4.05891075160112,5.32530464606164,-6.49781028429742));
#36779=CARTESIAN_POINT('Ctrl Pts',(-3.94147185709489,7.76293269109889,-3.21205294140231));
#36780=CARTESIAN_POINT('Ctrl Pts',(-3.82403296258866,8.35957156616068,0.835446762709816));
#36781=CARTESIAN_POINT('Ctrl Pts',(-3.70659406808243,6.97372761835372,4.68481922503354));
#36782=CARTESIAN_POINT('Ctrl Pts',(-3.58915517357619,3.93405546743286,7.42318096516021));
#36783=CARTESIAN_POINT('Ctrl Pts',(-3.47171627906997,-0.0385828430310631,
8.40112608093868));
#36784=CARTESIAN_POINT('Ctrl Pts',(-3.35427738456373,-4.00207118653311,
7.38673366869508));
#36785=CARTESIAN_POINT('Ctrl Pts',(-3.2368384900575,-7.01646335196947,4.620568153675));
#36786=CARTESIAN_POINT('Ctrl Pts',(-3.15135025156088,-7.99949209086729,
1.80931584281257));
#36787=CARTESIAN_POINT('Ctrl Pts',(-3.105008311233,-8.06892511888092,0.243355117950805));
#36788=CARTESIAN_POINT('Ctrl Pts',(-3.09781266907387,-8.06868808348557,
0.000183093833578535));
#36789=CARTESIAN_POINT('Ctrl Pts',(-4.30218733092611,-8.06885784129,0.000156365259223988));
#36790=CARTESIAN_POINT('Ctrl Pts',(-4.26848974516519,-8.06784839022042,
-1.13856225358147));
#36791=CARTESIAN_POINT('Ctrl Pts',(-4.19564586123552,-7.54138222205796,
-3.60102803550426));
#36792=CARTESIAN_POINT('Ctrl Pts',(-4.08365567913712,-5.12042931874465,
-6.66045126420618));
#36793=CARTESIAN_POINT('Ctrl Pts',(-3.96621678463087,-1.36737242671985,
-8.28919176391845));
#36794=CARTESIAN_POINT('Ctrl Pts',(-3.84877789012465,2.70995854408127,-7.9521400989076));
#36795=CARTESIAN_POINT('Ctrl Pts',(-3.73133899561841,6.14461946158279,-5.72922849019895));
#36796=CARTESIAN_POINT('Ctrl Pts',(-3.61390010111218,8.12207621918668,-2.14762320163677));
#36797=CARTESIAN_POINT('Ctrl Pts',(-3.49646120660595,8.17337245336549,1.94329361215914));
#36798=CARTESIAN_POINT('Ctrl Pts',(-3.37902231209972,6.28634325160488,5.57335591345347));
#36799=CARTESIAN_POINT('Ctrl Pts',(-3.26158341759348,2.90849983754228,7.88168992567818));
#36800=CARTESIAN_POINT('Ctrl Pts',(-3.14414452308725,-1.1590978033505,8.32087130825875));
#36801=CARTESIAN_POINT('Ctrl Pts',(-3.02670562858102,-4.95181422457809,
6.78674774808702));
#36802=CARTESIAN_POINT('Ctrl Pts',(-2.91271989786064,-7.49321035547616,
3.73557280180067));
#36803=CARTESIAN_POINT('Ctrl Pts',(-2.837880465309,-8.06820478007428,1.20597261551876));
#36804=CARTESIAN_POINT('Ctrl Pts',(-2.80218733092611,-8.06902159023132,
-0.000109298400165197));
#36805=CARTESIAN_POINT('Origin',(-14.3478126690739,0.,0.));
#36806=CARTESIAN_POINT('',(-6.09781266907388,-8.06804319777117,-0.000144302944734027));
#36807=CARTESIAN_POINT('',(-5.80218733092611,-8.06802936020891,0.00014009232313511));
#36808=CARTESIAN_POINT('',(-14.3478126690739,-8.0685,-1.61713948722842E-13));
#36809=CARTESIAN_POINT('Ctrl Pts',(-6.09781266907388,-8.06804319777117,
-0.000144302944733825));
#36810=CARTESIAN_POINT('Ctrl Pts',(-6.08366576545161,-8.06835928950991,
-0.478339617312313));
#36811=CARTESIAN_POINT('Ctrl Pts',(-6.0303725636606,-7.91071536051216,-2.27955671366496));
#36812=CARTESIAN_POINT('Ctrl Pts',(-5.93793306370085,-6.58660781722385,
-5.21507483420824));
#36813=CARTESIAN_POINT('Ctrl Pts',(-5.8204941691946,-3.34238556640572,-7.70771475794147));
#36814=CARTESIAN_POINT('Ctrl Pts',(-5.70305527468838,0.694487590192009,
-8.37246051357519));
#36815=CARTESIAN_POINT('Ctrl Pts',(-5.58561638018214,4.56666214859352,-7.0516668160733));
#36816=CARTESIAN_POINT('Ctrl Pts',(-5.46817748567591,7.35584708280132,-4.05856153812523));
#36817=CARTESIAN_POINT('Ctrl Pts',(-5.35073859116968,8.40058370692718,-0.102963329471767));
#36818=CARTESIAN_POINT('Ctrl Pts',(-5.23329969666345,7.45311142753807,3.87705276118435));
#36819=CARTESIAN_POINT('Ctrl Pts',(-5.11586080215721,4.73812447740229,6.93762095396888));
#36820=CARTESIAN_POINT('Ctrl Pts',(-4.99842190765099,0.89948539794352,8.35292368474611));
#36821=CARTESIAN_POINT('Ctrl Pts',(-4.88098301314475,-3.15246776549777,
7.7873201457114));
#36822=CARTESIAN_POINT('Ctrl Pts',(-4.76354411863852,-6.45680926651568,
5.37494392158168));
#36823=CARTESIAN_POINT('Ctrl Pts',(-4.66915400394823,-7.88191821152657,
2.41152062990943));
#36824=CARTESIAN_POINT('Ctrl Pts',(-4.61391018742668,-8.06817215353576,
0.544250997976407));
#36825=CARTESIAN_POINT('Ctrl Pts',(-4.59781266907387,-8.06793026735018,
9.89360780155601E-5));
#36826=CARTESIAN_POINT('Ctrl Pts',(-5.80218733092611,-8.06802936020891,
0.00014009232313518));
#36827=CARTESIAN_POINT('Ctrl Pts',(-5.77739162135886,-8.06749280865517,
-0.838011532852666));
#36828=CARTESIAN_POINT('Ctrl Pts',(-5.71344961362287,-7.73214656047648,
-2.99981704381613));
#36829=CARTESIAN_POINT('Ctrl Pts',(-5.61036130771812,-5.83193878421242,
-6.0472222937725));
#36830=CARTESIAN_POINT('Ctrl Pts',(-5.49292241321191,-2.28415769210351,
-8.08474063224692));
#36831=CARTESIAN_POINT('Ctrl Pts',(-5.37548351870566,1.80531424554574,-8.20495264629408));
#36832=CARTESIAN_POINT('Ctrl Pts',(-5.25804462419944,5.46665365823166,-6.37934990685156));
#36833=CARTESIAN_POINT('Ctrl Pts',(-5.14060572969319,7.83156933772,-3.0408763805148));
#36834=CARTESIAN_POINT('Ctrl Pts',(-5.02316683518698,8.3392185810425,1.01874477211711));
#36835=CARTESIAN_POINT('Ctrl Pts',(-4.90572794068073,6.86921173698437,4.83676933143891));
#36836=CARTESIAN_POINT('Ctrl Pts',(-4.78828904617451,3.770162762059,7.50774801126825));
#36837=CARTESIAN_POINT('Ctrl Pts',(-4.67085015166827,-0.222985014150146,
8.39825488638014));
#36838=CARTESIAN_POINT('Ctrl Pts',(-4.55341125716204,-4.16325161610056,
7.29710514066449));
#36839=CARTESIAN_POINT('Ctrl Pts',(-4.43597236265581,-7.1161979048615,4.46543780972854));
#36840=CARTESIAN_POINT('Ctrl Pts',(-4.3522310539105,-8.0184584470612,1.69115891412015));
#36841=CARTESIAN_POINT('Ctrl Pts',(-4.30763604333393,-8.06902106391987,
0.18428083968042));
#36842=CARTESIAN_POINT('Ctrl Pts',(-4.30218733092611,-8.06885784129,0.000156365259223988));
#36843=CARTESIAN_POINT('Origin',(-14.3478126690739,0.,0.));
#36844=CARTESIAN_POINT('',(-7.59781266907388,-8.06887641478357,-0.000152324058379699));
#36845=CARTESIAN_POINT('',(-7.30218733092611,-8.06793992440636,-0.000104148435049745));
#36846=CARTESIAN_POINT('',(-14.3478126690739,-8.0685,-1.61713948722842E-13));
#36847=CARTESIAN_POINT('Ctrl Pts',(-7.59781266907388,-8.06887641478357,
-0.000152324058379522));
#36848=CARTESIAN_POINT('Ctrl Pts',(-7.59256764164528,-8.06903072901403,
-0.177392638492444));
#36849=CARTESIAN_POINT('Ctrl Pts',(-7.54817631604794,-8.02058356892345,
-1.67738301722052));
#36850=CARTESIAN_POINT('Ctrl Pts',(-7.46463869228187,-7.12760426199033,
-4.44720873681053));
#36851=CARTESIAN_POINT('Ctrl Pts',(-7.34719979777563,-4.18191550738002,
-7.28642510106571));
#36852=CARTESIAN_POINT('Ctrl Pts',(-7.2297609032694,-0.244480274405397,
-8.39765666479245));
#36853=CARTESIAN_POINT('Ctrl Pts',(-7.11232200876316,3.75093376056635,-7.51737347669715));
#36854=CARTESIAN_POINT('Ctrl Pts',(-6.99488311425694,6.85680917596183,-4.85433579274776));
#36855=CARTESIAN_POINT('Ctrl Pts',(-6.8774442197507,8.33658374329481,-1.04008632109978));
#36856=CARTESIAN_POINT('Ctrl Pts',(-6.76000532524447,7.83932707831064,3.02082091881856));
#36857=CARTESIAN_POINT('Ctrl Pts',(-6.64256643073823,5.48296421930119,6.36533671019601));
#36858=CARTESIAN_POINT('Ctrl Pts',(-6.52512753623201,1.82630955719499,8.20030496174408));
#36859=CARTESIAN_POINT('Ctrl Pts',(-6.40768864172577,-2.26345669421878,
8.09056066399));
#36860=CARTESIAN_POINT('Ctrl Pts',(-6.29024974721954,-5.81644136755901,
6.06212981402202));
#36861=CARTESIAN_POINT('Ctrl Pts',(-6.18695775633558,-7.72821288647723,
3.01358673818511));
#36862=CARTESIAN_POINT('Ctrl Pts',(-6.12281206362035,-8.0674846230964,0.844888196982259));
#36863=CARTESIAN_POINT('Ctrl Pts',(-6.09781266907388,-8.06804319777117,
-0.000144302944733825));
#36864=CARTESIAN_POINT('Ctrl Pts',(-7.30218733092611,-8.06793992440636,
-0.000104148435049883));
#36865=CARTESIAN_POINT('Ctrl Pts',(-7.28629349755254,-8.06819173593772,
-0.537369098197992));
#36866=CARTESIAN_POINT('Ctrl Pts',(-7.23125336601021,-7.88500596100739,
-2.39774097328042));
#36867=CARTESIAN_POINT('Ctrl Pts',(-7.13706693629915,-6.47054567674393,
-5.35839958366958));
#36868=CARTESIAN_POINT('Ctrl Pts',(-7.01962804179292,-3.17238967957803,
-7.77922561531716));
#36869=CARTESIAN_POINT('Ctrl Pts',(-6.90218914728668,0.878102486783198,
-8.35519858984843));
#36870=CARTESIAN_POINT('Ctrl Pts',(-6.78475025278046,4.72035155321251,-6.94972579798543));
#36871=CARTESIAN_POINT('Ctrl Pts',(-6.66731135827422,7.4431633614575,-3.89611686525913));
#36872=CARTESIAN_POINT('Ctrl Pts',(-6.54987246376799,8.40081969523418,0.0814610413973314));
#36873=CARTESIAN_POINT('Ctrl Pts',(-6.43243356926176,7.36621116057458,4.03972036048615));
#36874=CARTESIAN_POINT('Ctrl Pts',(-6.31499467475553,4.58469646186278,7.03995495764589));
#36875=CARTESIAN_POINT('Ctrl Pts',(-6.1975557802493,0.715915279072651,8.3706554561928));
#36876=CARTESIAN_POINT('Ctrl Pts',(-6.08011688574306,-3.32264610505695,
7.71624457321371));
#36877=CARTESIAN_POINT('Ctrl Pts',(-5.96267799123684,-6.57323782128532,
5.23191666580462));
#36878=CARTESIAN_POINT('Ctrl Pts',(-5.87003480629784,-7.90778884858942,
2.29333657883371));
#36879=CARTESIAN_POINT('Ctrl Pts',(-5.8165379195276,-8.06833989097192,0.485222768660689));
#36880=CARTESIAN_POINT('Ctrl Pts',(-5.80218733092611,-8.06802936020891,
0.00014009232313518));
#36881=CARTESIAN_POINT('Origin',(-14.3478126690739,0.,0.));
#36882=CARTESIAN_POINT('',(-9.09781266907388,-8.0690069255314,0.000114842546288661));
#36883=CARTESIAN_POINT('',(-8.80218733092612,-8.06870858189138,-0.000180733618864171));
#36884=CARTESIAN_POINT('',(-14.3478126690739,-8.0685,-1.61713948722842E-13));
#36885=CARTESIAN_POINT('Ctrl Pts',(-9.09781266907388,-8.0690069255314,0.000114842546288605));
#36886=CARTESIAN_POINT('Ctrl Pts',(-9.06232321967021,-8.06816227230134,
-1.19909076398325));
#36887=CARTESIAN_POINT('Ctrl Pts',(-8.9876874720978,-7.4982202312652,-3.7218450346353));
#36888=CARTESIAN_POINT('Ctrl Pts',(-8.87390542635665,-4.96916911103115,
-6.77405096026056));
#36889=CARTESIAN_POINT('Ctrl Pts',(-8.75646653185041,-1.18039199564904,
-8.31787730131265));
#36890=CARTESIAN_POINT('Ctrl Pts',(-8.63902763734419,2.88831655372436,-7.88910866640744));
#36891=CARTESIAN_POINT('Ctrl Pts',(-8.52158874283795,6.27205722999723,-5.5894280716122));
#36892=CARTESIAN_POINT('Ctrl Pts',(-8.40414984833172,8.16837171151259,-1.96420763844087));
#36893=CARTESIAN_POINT('Ctrl Pts',(-8.28671095382549,8.12754665384501,2.12682708603627));
#36894=CARTESIAN_POINT('Ctrl Pts',(-8.16927205931926,6.15926377034014,5.71348211440747));
#36895=CARTESIAN_POINT('Ctrl Pts',(-8.05183316481303,2.73030380171169,7.94517773336033));
#36896=CARTESIAN_POINT('Ctrl Pts',(-7.93439427030679,-1.34615111879544,
8.29266454341796));
#36897=CARTESIAN_POINT('Ctrl Pts',(-7.81695537580056,-5.1033646225271,6.67353561418904));
#36898=CARTESIAN_POINT('Ctrl Pts',(-7.70476150872293,-7.53655783590869,
3.61476589733093));
#36899=CARTESIAN_POINT('Ctrl Pts',(-7.63171393981403,-8.06787900369719,
1.14544166329457));
#36900=CARTESIAN_POINT('Ctrl Pts',(-7.59781266907388,-8.06887641478357,
-0.000152324058379522));
#36901=CARTESIAN_POINT('Ctrl Pts',(-8.80218733092612,-8.06870858189138,
-0.000180733618863893));
#36902=CARTESIAN_POINT('Ctrl Pts',(-8.79519537374621,-8.06893746644687,
-0.236467619644774));
#36903=CARTESIAN_POINT('Ctrl Pts',(-8.74905711839756,-8.00177191450951,
-1.79553866882014));
#36904=CARTESIAN_POINT('Ctrl Pts',(-8.66377256488016,-7.02826704496481,
-4.60259381194273));
#36905=CARTESIAN_POINT('Ctrl Pts',(-8.54633367037395,-4.02096498037294,
-7.37646582583656));
#36906=CARTESIAN_POINT('Ctrl Pts',(-8.4288947758677,-0.0600860556372529,
-8.400999769016));
#36907=CARTESIAN_POINT('Ctrl Pts',(-8.31145588136148,3.91504235213327,-7.43322613904));
#36908=CARTESIAN_POINT('Ctrl Pts',(-8.19401698685524,6.96171358315727,-4.70265365928452));
#36909=CARTESIAN_POINT('Ctrl Pts',(-8.07657809234901,8.35740575511295,-0.856840998963709));
#36910=CARTESIAN_POINT('Ctrl Pts',(-7.95913919784278,7.77112872867905,3.19217257293514));
#36911=CARTESIAN_POINT('Ctrl Pts',(-7.84170030333654,5.34191883189369,6.48415843780511));
#36912=CARTESIAN_POINT('Ctrl Pts',(-7.72426140883031,1.64586622155058,8.23841804194586));
#36913=CARTESIAN_POINT('Ctrl Pts',(-7.60682251432408,-2.44050561599858,
8.038926532279));
#36914=CARTESIAN_POINT('Ctrl Pts',(-7.48938361981785,-5.94810850285432,
5.93299356913289));
#36915=CARTESIAN_POINT('Ctrl Pts',(-7.38783855868519,-7.76130804072777,
2.895476037464));
#36916=CARTESIAN_POINT('Ctrl Pts',(-7.32543979572128,-8.06757152751744,
0.785907258404543));
#36917=CARTESIAN_POINT('Ctrl Pts',(-7.30218733092611,-8.06793992440636,
-0.000104148435049883));
#36918=CARTESIAN_POINT('Origin',(-14.3478126690739,0.,0.));
#36919=CARTESIAN_POINT('',(-10.5978126690739,-8.06816497465237,0.000173167597293405));
#36920=CARTESIAN_POINT('',(-10.3021873309261,-8.06911057618467,6.34335902039915E-5));
#36921=CARTESIAN_POINT('',(-14.3478126690739,-8.0685,-1.61713948722842E-13));
#36922=CARTESIAN_POINT('Ctrl Pts',(-10.5978126690739,-8.06816497465237,
0.000173167597293036));
#36923=CARTESIAN_POINT('Ctrl Pts',(-10.5712250958639,-8.06744060058938,
-0.898504524201405));
#36924=CARTESIAN_POINT('Ctrl Pts',(-10.5054912244852,-7.69685793866654,
-3.12093756422147));
#36925=CARTESIAN_POINT('Ctrl Pts',(-10.4006110549377,-5.69430528428376,
-6.17699632956363));
#36926=CARTESIAN_POINT('Ctrl Pts',(-10.2831721604314,-2.10154812737837,
-8.1341202063368));
#36927=CARTESIAN_POINT('Ctrl Pts',(-10.1657332659252,1.98959372976295,-8.16222523101317));
#36928=CARTESIAN_POINT('Ctrl Pts',(-10.048294371419,5.60890098251375,-6.25464942822609));
#36929=CARTESIAN_POINT('Ctrl Pts',(-9.93085547691274,7.89805035642209,-2.86377517127619));
#36930=CARTESIAN_POINT('Ctrl Pts',(-9.8134165824065,8.31416724541664,1.20624666449639));
#36931=CARTESIAN_POINT('Ctrl Pts',(-9.69597768790028,6.75856899858617,4.99020573884583));
#36932=CARTESIAN_POINT('Ctrl Pts',(-9.57853879339404,3.60016768628482,7.59073122748412));
#36933=CARTESIAN_POINT('Ctrl Pts',(-9.46109989888781,-0.412017884052814,
8.3911053741381));
#36934=CARTESIAN_POINT('Ctrl Pts',(-9.34366100438158,-4.32649289879303,
7.20151839746173));
#36935=CARTESIAN_POINT('Ctrl Pts',(-9.22622210987535,-7.21493472673645,
4.30408236018371));
#36936=CARTESIAN_POINT('Ctrl Pts',(-9.14427266477278,-8.03653802371325,
1.56997461945975));
#36937=CARTESIAN_POINT('Ctrl Pts',(-9.10146951783896,-8.06909395897861,
0.123681525461907));
#36938=CARTESIAN_POINT('Ctrl Pts',(-9.09781266907388,-8.0690069255314,0.000114842546288605));
#36939=CARTESIAN_POINT('Ctrl Pts',(-10.3021873309261,-8.06911057618467,
6.34335902037139E-5));
#36940=CARTESIAN_POINT('Ctrl Pts',(-10.2649509517711,-8.0685730995522,-1.25812477433403));
#36941=CARTESIAN_POINT('Ctrl Pts',(-10.1885682744474,-7.45456459945451,
-3.839542418202));
#36942=CARTESIAN_POINT('Ctrl Pts',(-10.073039298955,-4.81927591637304,-6.88149598316814));
#36943=CARTESIAN_POINT('Ctrl Pts',(-9.95560040444872,-0.997523488572918,
-8.34178364717233));
#36944=CARTESIAN_POINT('Ctrl Pts',(-9.83816150994251,3.06079288122268,-7.82380689682625));
#36945=CARTESIAN_POINT('Ctrl Pts',(-9.72072261543626,6.39323840044666,-5.45040459216995));
#36946=CARTESIAN_POINT('Ctrl Pts',(-9.60328372093004,8.20951945985529,-1.78443203586594));
#36947=CARTESIAN_POINT('Ctrl Pts',(-9.48584482642378,8.07890273990855,2.30472080092658));
#36948=CARTESIAN_POINT('Ctrl Pts',(-9.36840593191757,6.03236415915333,5.84730622649608));
#36949=CARTESIAN_POINT('Ctrl Pts',(-9.25096703741134,2.55524289425404,8.00319568692536));
#36950=CARTESIAN_POINT('Ctrl Pts',(-9.1335281429051,-1.5278574099364,8.26111730873075));
#36951=CARTESIAN_POINT('Ctrl Pts',(-9.01608924839887,-5.24862442380086,
6.55990465713925));
#36952=CARTESIAN_POINT('Ctrl Pts',(-8.90564231107254,-7.57725711709514,
3.49690855884589));
#36953=CARTESIAN_POINT('Ctrl Pts',(-8.83434167191496,-8.06765599649145,
1.08644621631508));
#36954=CARTESIAN_POINT('Ctrl Pts',(-8.80218733092612,-8.06870858189138,
-0.000180733618863893));
#36955=CARTESIAN_POINT('Origin',(9.5,-11.,5.85085296108588));
#36956=CARTESIAN_POINT('',(9.5,-10.5669872981078,6.60085296108588));
#36957=CARTESIAN_POINT('',(10.,-10.5,6.06217782649107));
#36958=CARTESIAN_POINT('',(9.5,-10.5669872981078,6.60085296108588));
#36959=CARTESIAN_POINT('',(9.5,-11.,5.85085296108588));
#36960=CARTESIAN_POINT('',(9.5,-11.,5.85085296108588));
#36961=CARTESIAN_POINT('',(10.,-10.5,6.06217782649107));
#36962=CARTESIAN_POINT('Origin',(2.,-10.7834936490539,6.22585296108588));
#36963=CARTESIAN_POINT('',(2.,-11.,5.85085296108588));
#36964=CARTESIAN_POINT('',(2.,-10.5669872981078,6.60085296108588));
#36965=CARTESIAN_POINT('',(2.,-10.7834936490539,6.22585296108588));
#36966=CARTESIAN_POINT('',(2.,-11.,5.85085296108588));
#36967=CARTESIAN_POINT('',(2.,-10.5669872981078,6.60085296108588));
#36968=CARTESIAN_POINT('Origin',(9.5,-0.433012701892219,12.4517059221718));
#36969=CARTESIAN_POINT('',(9.5,0.433012701892219,12.4517059221718));
#36970=CARTESIAN_POINT('',(10.,-1.11022302462516E-15,12.1243556529821));
#36971=CARTESIAN_POINT('',(9.5,0.433012701892218,12.4517059221718));
#36972=CARTESIAN_POINT('',(9.5,-0.433012701892218,12.4517059221718));
#36973=CARTESIAN_POINT('',(9.5,-0.433012701892219,12.4517059221718));
#36974=CARTESIAN_POINT('',(10.,1.38777878078145E-15,12.1243556529821));
#36975=CARTESIAN_POINT('Origin',(2.,1.73472347597681E-16,12.4517059221718));
#36976=CARTESIAN_POINT('',(2.,-0.433012701892219,12.4517059221718));
#36977=CARTESIAN_POINT('',(2.,0.433012701892219,12.4517059221718));
#36978=CARTESIAN_POINT('',(2.,8.67361737988404E-17,12.4517059221718));
#36979=CARTESIAN_POINT('',(2.,-0.433012701892219,12.4517059221718));
#36980=CARTESIAN_POINT('',(2.,0.433012701892219,12.4517059221718));
#36981=CARTESIAN_POINT('Origin',(9.75,-2.625,10.8974863309542));
#36982=CARTESIAN_POINT('',(10.,-2.5,10.6809799800081));
#36983=CARTESIAN_POINT('',(9.5,-2.75,11.1139926819003));
#36984=CARTESIAN_POINT('Origin',(9.5,-10.5669872981078,-6.60085296108588));
#36985=CARTESIAN_POINT('',(9.5,-11.,-5.85085296108588));
#36986=CARTESIAN_POINT('',(10.,-10.5,-6.06217782649107));
#36987=CARTESIAN_POINT('',(9.5,-11.,-5.85085296108588));
#36988=CARTESIAN_POINT('',(9.5,-10.5669872981078,-6.60085296108589));
#36989=CARTESIAN_POINT('',(9.5,-10.5669872981078,-6.60085296108588));
#36990=CARTESIAN_POINT('',(10.,-10.5,-6.06217782649107));
#36991=CARTESIAN_POINT('Origin',(2.,-10.7834936490539,-6.22585296108588));
#36992=CARTESIAN_POINT('',(2.,-10.5669872981078,-6.60085296108588));
#36993=CARTESIAN_POINT('',(2.,-11.,-5.85085296108588));
#36994=CARTESIAN_POINT('',(2.,-10.7834936490539,-6.22585296108588));
#36995=CARTESIAN_POINT('',(2.,-10.5669872981078,-6.60085296108588));
#36996=CARTESIAN_POINT('',(2.,-11.,-5.85085296108588));
#36997=CARTESIAN_POINT('Origin',(9.5,10.5669872981078,6.60085296108588));
#36998=CARTESIAN_POINT('',(9.5,11.,5.85085296108588));
#36999=CARTESIAN_POINT('',(10.,10.5,6.06217782649107));
#37000=CARTESIAN_POINT('',(9.5,11.,5.85085296108588));
#37001=CARTESIAN_POINT('',(9.5,10.5669872981078,6.60085296108588));
#37002=CARTESIAN_POINT('',(9.5,10.5669872981078,6.60085296108588));
#37003=CARTESIAN_POINT('',(10.,10.5,6.06217782649107));
#37004=CARTESIAN_POINT('Origin',(2.,10.7834936490539,6.22585296108588));
#37005=CARTESIAN_POINT('',(2.,10.5669872981078,6.60085296108588));
#37006=CARTESIAN_POINT('',(2.,11.,5.85085296108588));
#37007=CARTESIAN_POINT('',(2.,10.7834936490539,6.22585296108588));
#37008=CARTESIAN_POINT('',(2.,10.5669872981078,6.60085296108588));
#37009=CARTESIAN_POINT('',(2.,11.,5.85085296108588));
#37010=CARTESIAN_POINT('Origin',(9.75,8.125,7.72205985041124));
#37011=CARTESIAN_POINT('',(10.,8.,7.50555349946513));
#37012=CARTESIAN_POINT('',(9.5,8.25,7.93856620135735));
#37013=CARTESIAN_POINT('Origin',(9.5,0.433012701892216,-12.4517059221718));
#37014=CARTESIAN_POINT('',(9.5,-0.433012701892221,-12.4517059221718));
#37015=CARTESIAN_POINT('',(10.,-2.22044604925031E-15,-12.1243556529821));
#37016=CARTESIAN_POINT('',(9.5,-0.43301270189222,-12.4517059221718));
#37017=CARTESIAN_POINT('',(9.5,0.433012701892216,-12.4517059221718));
#37018=CARTESIAN_POINT('',(9.5,0.433012701892216,-12.4517059221718));
#37019=CARTESIAN_POINT('',(10.,-2.22044604925031E-15,-12.1243556529821));
#37020=CARTESIAN_POINT('Origin',(2.,-2.18575157973078E-15,-12.4517059221718));
#37021=CARTESIAN_POINT('',(2.,0.433012701892215,-12.4517059221718));
#37022=CARTESIAN_POINT('',(2.,-0.433012701892219,-12.4517059221718));
#37023=CARTESIAN_POINT('',(2.,-1.09287578986539E-15,-12.4517059221718));
#37024=CARTESIAN_POINT('',(2.,0.433012701892216,-12.4517059221718));
#37025=CARTESIAN_POINT('',(2.,-0.433012701892221,-12.4517059221718));
#37026=CARTESIAN_POINT('Origin',(9.5,11.,-5.85085296108589));
#37027=CARTESIAN_POINT('',(9.5,10.5669872981078,-6.60085296108589));
#37028=CARTESIAN_POINT('',(10.,10.5,-6.06217782649107));
#37029=CARTESIAN_POINT('',(9.5,10.5669872981078,-6.60085296108589));
#37030=CARTESIAN_POINT('',(9.5,11.,-5.85085296108589));
#37031=CARTESIAN_POINT('',(9.5,11.,-5.85085296108589));
#37032=CARTESIAN_POINT('',(10.,10.5,-6.06217782649108));
#37033=CARTESIAN_POINT('Origin',(2.,10.7834936490539,-6.22585296108589));
#37034=CARTESIAN_POINT('',(2.,11.,-5.85085296108589));
#37035=CARTESIAN_POINT('',(2.,10.5669872981078,-6.60085296108589));
#37036=CARTESIAN_POINT('',(2.,10.7834936490539,-6.22585296108588));
#37037=CARTESIAN_POINT('',(2.,11.,-5.85085296108589));
#37038=CARTESIAN_POINT('',(2.,10.5669872981078,-6.60085296108589));
#37039=CARTESIAN_POINT('Origin',(9.75,10.75,-3.17542648054295));
#37040=CARTESIAN_POINT('',(10.,10.5,-3.17542648054295));
#37041=CARTESIAN_POINT('',(9.5,11.,-3.17542648054295));
#37042=CARTESIAN_POINT('Origin',(9.75,2.625,-10.8974863309542));
#37043=CARTESIAN_POINT('',(10.,2.5,-10.6809799800081));
#37044=CARTESIAN_POINT('',(9.5,2.75,-11.1139926819003));
#37045=CARTESIAN_POINT('Origin',(9.75,-8.125,-7.72205985041125));
#37046=CARTESIAN_POINT('',(10.,-8.,-7.50555349946514));
#37047=CARTESIAN_POINT('',(9.5,-8.25,-7.93856620135736));
#37048=CARTESIAN_POINT('Origin',(9.75,-10.75,3.17542648054294));
#37049=CARTESIAN_POINT('',(10.,-10.5,3.17542648054294));
#37050=CARTESIAN_POINT('',(9.5,-11.,3.17542648054294));
#37051=CARTESIAN_POINT('Origin',(2.,7.77755175064932E-16,12.7017059221718));
#37052=CARTESIAN_POINT('',(2.,-2.75,11.1139926819003));
#37053=CARTESIAN_POINT('Origin',(2.,11.,6.35085296108588));
#37054=CARTESIAN_POINT('',(2.,8.25,7.93856620135735));
#37055=CARTESIAN_POINT('Origin',(2.,11.,-6.35085296108589));
#37056=CARTESIAN_POINT('',(2.,11.,-3.17542648054295));
#37057=CARTESIAN_POINT('Origin',(10.,0.,0.));
#37058=CARTESIAN_POINT('',(10.,4.5,2.59807621135332));
#37059=CARTESIAN_POINT('',(10.,0.,5.19615242270663));
#37060=CARTESIAN_POINT('',(10.,1.25,4.4744645862196));
#37061=CARTESIAN_POINT('',(10.,4.5,-2.59807621135332));
#37062=CARTESIAN_POINT('',(10.,4.5,1.15470053837925));
#37063=CARTESIAN_POINT('',(10.,-5.55111512312578E-16,-5.19615242270663));
#37064=CARTESIAN_POINT('',(10.,3.25,-3.31976404784035));
#37065=CARTESIAN_POINT('',(10.,-4.5,-2.59807621135332));
#37066=CARTESIAN_POINT('',(10.,-1.25,-4.4744645862196));
#37067=CARTESIAN_POINT('',(10.,-4.5,2.59807621135332));
#37068=CARTESIAN_POINT('',(10.,-4.5,-1.15470053837925));
#37069=CARTESIAN_POINT('',(10.,-3.25,3.31976404784035));
#37070=CARTESIAN_POINT('Origin',(9.75,-1.125,-4.25795823527349));
#37071=CARTESIAN_POINT('',(9.5,-8.48460190979926E-16,-4.61880215351701));
#37072=CARTESIAN_POINT('',(10.,-1.11022302462516E-15,-5.19615242270663));
#37073=CARTESIAN_POINT('',(9.5,-4.,-2.3094010767585));
#37074=CARTESIAN_POINT('',(9.5,-1.,-4.04145188432738));
#37075=CARTESIAN_POINT('',(10.,-4.5,-2.59807621135332));
#37076=CARTESIAN_POINT('Origin',(9.75,3.125,-3.10325769689424));
#37077=CARTESIAN_POINT('',(9.5,4.,-2.30940107675851));
#37078=CARTESIAN_POINT('',(10.,4.5,-2.59807621135332));
#37079=CARTESIAN_POINT('',(9.5,3.,-2.88675134594813));
#37080=CARTESIAN_POINT('Origin',(9.75,1.125,4.25795823527349));
#37081=CARTESIAN_POINT('',(9.5,2.82820063659975E-16,4.61880215351701));
#37082=CARTESIAN_POINT('',(10.,0.,5.19615242270663));
#37083=CARTESIAN_POINT('',(9.5,4.,2.3094010767585));
#37084=CARTESIAN_POINT('',(9.5,1.,4.04145188432738));
#37085=CARTESIAN_POINT('',(9.5,4.,2.3094010767585));
#37086=CARTESIAN_POINT('Origin',(9.75,-3.125,3.10325769689424));
#37087=CARTESIAN_POINT('',(9.5,-4.,2.3094010767585));
#37088=CARTESIAN_POINT('',(9.5,-3.,2.88675134594813));
#37089=CARTESIAN_POINT('',(10.,-4.5,2.59807621135332));
#37090=CARTESIAN_POINT('Origin',(9.75,4.25,1.15470053837925));
#37091=CARTESIAN_POINT('',(9.5,4.,1.15470053837925));
#37092=CARTESIAN_POINT('Origin',(9.75,-4.25,-1.15470053837925));
#37093=CARTESIAN_POINT('',(9.5,-4.,-1.15470053837925));
#37094=CARTESIAN_POINT('Origin',(10.,4.,-2.30940107675851));
#37095=CARTESIAN_POINT('',(5.,4.,-2.30940107675851));
#37096=CARTESIAN_POINT('',(10.,4.,-2.30940107675851));
#37097=CARTESIAN_POINT('',(5.,-1.11022302462516E-15,-4.61880215351701));
#37098=CARTESIAN_POINT('',(5.,-8.48460190979926E-16,-4.61880215351701));
#37099=CARTESIAN_POINT('',(10.,-8.48460190979926E-16,-4.61880215351701));
#37100=CARTESIAN_POINT('Origin',(10.,4.,2.3094010767585));
#37101=CARTESIAN_POINT('',(5.,4.,2.3094010767585));
#37102=CARTESIAN_POINT('',(10.,4.,2.3094010767585));
#37103=CARTESIAN_POINT('',(5.,4.,-2.30940107675851));
#37104=CARTESIAN_POINT('Origin',(10.,5.55111512312578E-16,4.61880215351701));
#37105=CARTESIAN_POINT('',(5.,5.55111512312578E-16,4.61880215351701));
#37106=CARTESIAN_POINT('',(10.,2.82820063659975E-16,4.61880215351701));
#37107=CARTESIAN_POINT('',(5.,4.,2.3094010767585));
#37108=CARTESIAN_POINT('Ctrl Pts',(-12.0695005055609,-3.51734582803218,
7.26147165359919));
#37109=CARTESIAN_POINT('Ctrl Pts',(-12.0303542073922,-4.70805021950285,
6.68471265438406));
#37110=CARTESIAN_POINT('Ctrl Pts',(-11.9520616110547,-6.79926924260069,
4.93500196856942));
#37111=CARTESIAN_POINT('Ctrl Pts',(-11.8346227165485,-8.32382364819228,
1.13769958140006));
#37112=CARTESIAN_POINT('Ctrl Pts',(-11.7171838220422,-7.87424867921618,
-2.928432376846));
#37113=CARTESIAN_POINT('Ctrl Pts',(-11.599744927536,-5.55735101149824,-6.30056026334087));
#37114=CARTESIAN_POINT('Ctrl Pts',(-11.4823060330297,-1.92248730937921,
-8.17826163021399));
#37115=CARTESIAN_POINT('Ctrl Pts',(-11.3648671385235,2.16827971646752,-8.11660023363346));
#37116=CARTESIAN_POINT('Ctrl Pts',(-11.2474282440173,5.74484511045451,-6.13001490910025));
#37117=CARTESIAN_POINT('Ctrl Pts',(-11.129989349511,7.95900894851219,-2.68972043029039));
#37118=CARTESIAN_POINT('Ctrl Pts',(-11.0125504550048,8.28568610932253,1.38846061981056));
#37119=CARTESIAN_POINT('Ctrl Pts',(-10.8951115604986,6.64740134656684,5.1373583652959));
#37120=CARTESIAN_POINT('Ctrl Pts',(-10.7776726659924,3.43267763704583,7.66792930081125));
#37121=CARTESIAN_POINT('Ctrl Pts',(-10.6602337714861,-0.596110146715297,
8.38003913890674));
#37122=CARTESIAN_POINT('Ctrl Pts',(-10.5427948769799,-4.48352951771318,
7.10481331033355));
#37123=CARTESIAN_POINT('Ctrl Pts',(-10.4253559824737,-7.3076743467974,4.14467160188776));
#37124=CARTESIAN_POINT('Ctrl Pts',(-10.3079170879674,-8.3987950520306,0.201616129083312));
#37125=CARTESIAN_POINT('Ctrl Pts',(-10.1904781934612,-7.4981310548925,-3.78925300008877));
#37126=CARTESIAN_POINT('Ctrl Pts',(-10.073039298955,-4.81927591637304,-6.88149598316814));
#37127=CARTESIAN_POINT('Ctrl Pts',(-9.95560040444872,-0.997523488572918,
-8.34178364717233));
#37128=CARTESIAN_POINT('Ctrl Pts',(-9.83816150994251,3.06079288122268,-7.82380689682625));
#37129=CARTESIAN_POINT('Ctrl Pts',(-9.72072261543626,6.39323840044666,-5.45040459216995));
#37130=CARTESIAN_POINT('Ctrl Pts',(-9.60328372093004,8.20951945985529,-1.78443203586594));
#37131=CARTESIAN_POINT('Ctrl Pts',(-9.48584482642378,8.07890273990855,2.30472080092658));
#37132=CARTESIAN_POINT('Ctrl Pts',(-9.36840593191757,6.03236415915333,5.84730622649608));
#37133=CARTESIAN_POINT('Ctrl Pts',(-9.25096703741134,2.55524289425404,8.00319568692536));
#37134=CARTESIAN_POINT('Ctrl Pts',(-9.1335281429051,-1.5278574099364,8.26111730873075));
#37135=CARTESIAN_POINT('Ctrl Pts',(-9.01608924839887,-5.24862442380086,
6.55990465713925));
#37136=CARTESIAN_POINT('Ctrl Pts',(-8.89865035389263,-7.7246736093346,3.30300243451213));
#37137=CARTESIAN_POINT('Ctrl Pts',(-8.78121145938641,-8.36880681401512,
-0.737210935087755));
#37138=CARTESIAN_POINT('Ctrl Pts',(-8.66377256488016,-7.02826704496481,
-4.60259381194273));
#37139=CARTESIAN_POINT('Ctrl Pts',(-8.54633367037395,-4.02096498037294,
-7.37646582583656));
#37140=CARTESIAN_POINT('Ctrl Pts',(-8.4288947758677,-0.0600860556372529,
-8.400999769016));
#37141=CARTESIAN_POINT('Ctrl Pts',(-8.31145588136148,3.91504235213327,-7.43322613904));
#37142=CARTESIAN_POINT('Ctrl Pts',(-8.19401698685524,6.96171358315727,-4.70265365928452));
#37143=CARTESIAN_POINT('Ctrl Pts',(-8.07657809234901,8.35740575511295,-0.856840998963709));
#37144=CARTESIAN_POINT('Ctrl Pts',(-7.95913919784278,7.77112872867905,3.19217257293514));
#37145=CARTESIAN_POINT('Ctrl Pts',(-7.84170030333654,5.34191883189369,6.48415843780511));
#37146=CARTESIAN_POINT('Ctrl Pts',(-7.72426140883031,1.64586622155058,8.23841804194586));
#37147=CARTESIAN_POINT('Ctrl Pts',(-7.60682251432408,-2.44050561599858,
8.038926532279));
#37148=CARTESIAN_POINT('Ctrl Pts',(-7.48938361981785,-5.94810850285432,
5.93299356913289));
#37149=CARTESIAN_POINT('Ctrl Pts',(-7.37194472531161,-8.04511003962913,
2.42004378128959));
#37150=CARTESIAN_POINT('Ctrl Pts',(-7.25450583080538,-8.23420369644436,
-1.66682240762538));
#37151=CARTESIAN_POINT('Ctrl Pts',(-7.13706693629915,-6.47054567674393,
-5.35839958366958));
#37152=CARTESIAN_POINT('Ctrl Pts',(-7.01962804179292,-3.17238967957803,
-7.77922561531716));
#37153=CARTESIAN_POINT('Ctrl Pts',(-6.90218914728668,0.878102486783198,
-8.35519858984843));
#37154=CARTESIAN_POINT('Ctrl Pts',(-6.78475025278046,4.72035155321251,-6.94972579798543));
#37155=CARTESIAN_POINT('Ctrl Pts',(-6.66731135827422,7.4431633614575,-3.89611686525913));
#37156=CARTESIAN_POINT('Ctrl Pts',(-6.54987246376799,8.40081969523418,0.0814610413973314));
#37157=CARTESIAN_POINT('Ctrl Pts',(-6.43243356926176,7.36621116057458,4.03972036048615));
#37158=CARTESIAN_POINT('Ctrl Pts',(-6.31499467475553,4.58469646186278,7.03995495764589));
#37159=CARTESIAN_POINT('Ctrl Pts',(-6.1975557802493,0.715915279072651,8.3706554561928));
#37160=CARTESIAN_POINT('Ctrl Pts',(-6.08011688574306,-3.32264610505695,
7.71624457321371));
#37161=CARTESIAN_POINT('Ctrl Pts',(-5.96267799123684,-6.57323782128532,
5.23191666580462));
#37162=CARTESIAN_POINT('Ctrl Pts',(-5.84523909673059,-8.26497798989004,
1.50683319572324));
#37163=CARTESIAN_POINT('Ctrl Pts',(-5.72780020222437,-7.99666831990594,
-2.5755976460838));
#37164=CARTESIAN_POINT('Ctrl Pts',(-5.61036130771812,-5.83193878421242,
-6.0472222937725));
#37165=CARTESIAN_POINT('Ctrl Pts',(-5.49292241321191,-2.28415769210351,
-8.08474063224692));
#37166=CARTESIAN_POINT('Ctrl Pts',(-5.37548351870566,1.80531424554574,-8.20495264629408));
#37167=CARTESIAN_POINT('Ctrl Pts',(-5.25804462419944,5.46665365823166,-6.37934990685156));
#37168=CARTESIAN_POINT('Ctrl Pts',(-5.14060572969319,7.83156933772,-3.0408763805148));
#37169=CARTESIAN_POINT('Ctrl Pts',(-5.02316683518698,8.3392185810425,1.01874477211711));
#37170=CARTESIAN_POINT('Ctrl Pts',(-4.90572794068073,6.86921173698437,4.83676933143891));
#37171=CARTESIAN_POINT('Ctrl Pts',(-4.78828904617451,3.770162762059,7.50774801126825));
#37172=CARTESIAN_POINT('Ctrl Pts',(-4.67085015166827,-0.222985014150146,
8.39825488638014));
#37173=CARTESIAN_POINT('Ctrl Pts',(-4.55341125716204,-4.16325161610056,
7.29710514066449));
#37174=CARTESIAN_POINT('Ctrl Pts',(-4.43597236265581,-7.1161979048615,4.46543780972854));
#37175=CARTESIAN_POINT('Ctrl Pts',(-4.31853346814957,-8.3815289848282,0.574786332771845));
#37176=CARTESIAN_POINT('Ctrl Pts',(-4.20109457364334,-7.65917001270053,
-3.4521764398139));
#37177=CARTESIAN_POINT('Ctrl Pts',(-4.08365567913712,-5.12042931874465,
-6.66045126420618));
#37178=CARTESIAN_POINT('Ctrl Pts',(-3.96621678463087,-1.36737242671985,
-8.28919176391845));
#37179=CARTESIAN_POINT('Ctrl Pts',(-3.84877789012465,2.70995854408127,-7.9521400989076));
#37180=CARTESIAN_POINT('Ctrl Pts',(-3.73133899561841,6.14461946158279,-5.72922849019895));
#37181=CARTESIAN_POINT('Ctrl Pts',(-3.61390010111218,8.12207621918668,-2.14762320163677));
#37182=CARTESIAN_POINT('Ctrl Pts',(-3.49646120660595,8.17337245336549,1.94329361215914));
#37183=CARTESIAN_POINT('Ctrl Pts',(-3.37902231209972,6.28634325160488,5.57335591345347));
#37184=CARTESIAN_POINT('Ctrl Pts',(-3.26158341759348,2.90849983754228,7.88168992567818));
#37185=CARTESIAN_POINT('Ctrl Pts',(-3.14414452308725,-1.1590978033505,8.32087130825875));
#37186=CARTESIAN_POINT('Ctrl Pts',(-3.02670562858102,-4.95181422457809,
6.78674774808702));
#37187=CARTESIAN_POINT('Ctrl Pts',(-2.90926673407478,-7.57020119484931,
3.64313836494415));
#37188=CARTESIAN_POINT('Ctrl Pts',(-2.79182783956855,-8.39330655635519,
-0.364445569542508));
#37189=CARTESIAN_POINT('Ctrl Pts',(-2.67438894506232,-7.2259267400895,-4.28560128601273));
#37190=CARTESIAN_POINT('Ctrl Pts',(-2.55695005055609,-4.34491343911961,
-7.1904203216184));
#37191=CARTESIAN_POINT('Ctrl Pts',(-2.43951115604986,-0.433490517027392,
-8.39002416011216));
#37192=CARTESIAN_POINT('Ctrl Pts',(-2.32207226154363,3.58071951422406,-7.59991946597854));
#37193=CARTESIAN_POINT('Ctrl Pts',(-2.20463336703739,6.74578836548944,-5.00749194802054));
#37194=CARTESIAN_POINT('Ctrl Pts',(-2.08719447253116,8.31102423036551,-1.22751659427962));
#37195=CARTESIAN_POINT('Ctrl Pts',(-1.96975557802493,7.90541015591722,2.84353655923596));
#37196=CARTESIAN_POINT('Ctrl Pts',(-1.8523166835187,5.62478208560713,6.24029926664823));
#37197=CARTESIAN_POINT('Ctrl Pts',(-1.73487778901246,2.01069766784778,8.15705187872645));
#37198=CARTESIAN_POINT('Ctrl Pts',(-1.61743889450623,-2.08118048114745,
8.1395942446814));
#37199=CARTESIAN_POINT('Ctrl Pts',(-1.53914629816874,-4.4785344754388,6.8406029773222));
#37200=CARTESIAN_POINT('Ctrl Pts',(-1.5,-5.45359047959038,5.94634704090849));
#37201=CARTESIAN_POINT('Ctrl Pts',(-11.9046670037073,-3.64180542199675,
7.5184153428974));
#37202=CARTESIAN_POINT('Ctrl Pts',(-11.8655207055385,-4.87464231687759,
6.92124800331219));
#37203=CARTESIAN_POINT('Ctrl Pts',(-11.7872281092011,-7.03985812142109,
5.10962464465874));
#37204=CARTESIAN_POINT('Ctrl Pts',(-11.6697892146948,-8.61835815294024,
1.17795653504568));
#37205=CARTESIAN_POINT('Ctrl Pts',(-11.5523503201886,-8.15287518946173,
-3.03205355099106));
#37206=CARTESIAN_POINT('Ctrl Pts',(-11.4349114256823,-5.75399520977336,
-6.52350256428699));
#37207=CARTESIAN_POINT('Ctrl Pts',(-11.3174725311761,-1.99051360011823,
-8.4676454928187));
#37208=CARTESIAN_POINT('Ctrl Pts',(-11.2000336366699,2.24500325356257,-8.40380223731473));
#37209=CARTESIAN_POINT('Ctrl Pts',(-11.0825947421636,5.94812369743286,-6.34692254454031));
#37210=CARTESIAN_POINT('Ctrl Pts',(-10.9651558476574,8.24063466020584,-2.78489489677709));
#37211=CARTESIAN_POINT('Ctrl Pts',(-10.8477169531512,8.5788711355618,1.43759063244685));
#37212=CARTESIAN_POINT('Ctrl Pts',(-10.7302780586449,6.88261645277555,5.31914132536183));
#37213=CARTESIAN_POINT('Ctrl Pts',(-10.6128391641387,3.5541412877091,7.93925529887552));
#37214=CARTESIAN_POINT('Ctrl Pts',(-10.4954002696325,-0.617203218152013,
8.67656280181284));
#37215=CARTESIAN_POINT('Ctrl Pts',(-10.3779613751263,-4.64217705781445,
7.35621371934393));
#37216=CARTESIAN_POINT('Ctrl Pts',(-10.26052248062,-7.56625289621931,4.2913288172734));
#37217=CARTESIAN_POINT('Ctrl Pts',(-10.1430835861138,-8.69598238392063,
0.208750219044679));
#37218=CARTESIAN_POINT('Ctrl Pts',(-10.0256446916076,-7.76344882352011,
-3.92333389883392));
#37219=CARTESIAN_POINT('Ctrl Pts',(-9.90820579710132,-4.98980368164843,
-7.12499441573858));
#37220=CARTESIAN_POINT('Ctrl Pts',(-9.79076690259509,-1.03282037845178,
-8.63695365786423));
#37221=CARTESIAN_POINT('Ctrl Pts',(-9.67332800808886,3.1690975682883,-8.10064854881163));
#37222=CARTESIAN_POINT('Ctrl Pts',(-9.55588911358262,6.61946007279314,-5.64326454272637));
#37223=CARTESIAN_POINT('Ctrl Pts',(-9.4384502190764,8.50000936575956,-1.84757330701173));
#37224=CARTESIAN_POINT('Ctrl Pts',(-9.32101132457016,8.36477083586739,2.38627224030993));
#37225=CARTESIAN_POINT('Ctrl Pts',(-9.20357243006393,6.24581646967428,6.05421035088903));
#37226=CARTESIAN_POINT('Ctrl Pts',(-9.08613353555769,2.64565893767098,8.28638492515022));
#37227=CARTESIAN_POINT('Ctrl Pts',(-8.96869464105146,-1.58191991108739,
8.55343297975294));
#37228=CARTESIAN_POINT('Ctrl Pts',(-8.85125574654523,-5.43434447994452,
6.79202373498684));
#37229=CARTESIAN_POINT('Ctrl Pts',(-8.73381685203899,-7.99800747752137,
3.41987759037174));
#37230=CARTESIAN_POINT('Ctrl Pts',(-8.61637795753277,-8.66493302649592,
-0.763296790199302));
#37231=CARTESIAN_POINT('Ctrl Pts',(-8.49893906302653,-7.27695890111372,
-4.76545438495005));
#37232=CARTESIAN_POINT('Ctrl Pts',(-8.38150016852031,-4.16324489632963,
-7.6374785287276));
#37233=CARTESIAN_POINT('Ctrl Pts',(-8.26406127401406,-0.0622121718775053,
-8.6982651137584));
#37234=CARTESIAN_POINT('Ctrl Pts',(-8.14662237950784,4.05357424672756,-7.69624727837146));
#37235=CARTESIAN_POINT('Ctrl Pts',(-8.0291834850016,7.20805047700265,-4.86905480196603));
#37236=CARTESIAN_POINT('Ctrl Pts',(-7.91174459049537,8.65312854659645,-0.887159906468719));
#37237=CARTESIAN_POINT('Ctrl Pts',(-7.79430569598914,8.04610638896758,3.30512606733595));
#37238=CARTESIAN_POINT('Ctrl Pts',(-7.6768668014829,5.53094006589079,6.71359727203618));
#37239=CARTESIAN_POINT('Ctrl Pts',(-7.55942790697667,1.70410440786188,8.52993051030745));
#37240=CARTESIAN_POINT('Ctrl Pts',(-7.44198901247044,-2.52686173589292,
8.32338008931757));
#37241=CARTESIAN_POINT('Ctrl Pts',(-7.32455011796421,-6.15857946741587,
6.14292969901917));
#37242=CARTESIAN_POINT('Ctrl Pts',(-7.20711122345797,-8.32978239710749,
2.5056758689835));
#37243=CARTESIAN_POINT('Ctrl Pts',(-7.08967232895176,-8.52556704221308,
-1.72580211852295));
#37244=CARTESIAN_POINT('Ctrl Pts',(-6.9722334344455,-6.69950282995833,-5.54800398115828));
#37245=CARTESIAN_POINT('Ctrl Pts',(-6.85479453993929,-3.28464316579227,
-8.05448978005325));
#37246=CARTESIAN_POINT('Ctrl Pts',(-6.73735564543304,0.909173721830177,
-8.65084328184839));
#37247=CARTESIAN_POINT('Ctrl Pts',(-6.61991675092682,4.8873789273765,-7.19563850980607));
#37248=CARTESIAN_POINT('Ctrl Pts',(-6.50247785642058,7.7065361246348,-4.03397909058373));
#37249=CARTESIAN_POINT('Ctrl Pts',(-6.38503896191435,8.69807866815224,0.084343501249706));
#37250=CARTESIAN_POINT('Ctrl Pts',(-6.26760006740812,7.62686100705708,4.18266392656644));
#37251=CARTESIAN_POINT('Ctrl Pts',(-6.15016117290189,4.74692374572742,7.28906038497536));
#37252=CARTESIAN_POINT('Ctrl Pts',(-6.03272227839565,0.741247597617024,
8.6668470819898));
#37253=CARTESIAN_POINT('Ctrl Pts',(-5.91528338388943,-3.44021634277074,
7.98928018400289));
#37254=CARTESIAN_POINT('Ctrl Pts',(-5.79784448938318,-6.80582868674692,
5.41704552595052));
#37255=CARTESIAN_POINT('Ctrl Pts',(-5.68040559487697,-8.55743026926212,
1.56015176514495));
#37256=CARTESIAN_POINT('Ctrl Pts',(-5.56296670037072,-8.27962659038162,
-2.6667339326249));
#37257=CARTESIAN_POINT('Ctrl Pts',(-5.4455278058645,-6.03829913903584,-6.26120035225574));
#37258=CARTESIAN_POINT('Ctrl Pts',(-5.32808891135826,-2.36498151575047,
-8.37081529922423));
#37259=CARTESIAN_POINT('Ctrl Pts',(-5.21065001685203,1.86919442365855,-8.49528095769237));
#37260=CARTESIAN_POINT('Ctrl Pts',(-5.0932111223458,5.66008857419189,-6.60508014151799));
#37261=CARTESIAN_POINT('Ctrl Pts',(-4.97577222783956,8.10868565995078,-3.14847633176188));
#37262=CARTESIAN_POINT('Ctrl Pts',(-4.85833333333333,8.63429782810052,1.05479256692895));
#37263=CARTESIAN_POINT('Ctrl Pts',(-4.7408944388271,7.11227549739945,5.00791609281038));
#37264=CARTESIAN_POINT('Ctrl Pts',(-4.62345554432086,3.9035681618939,7.77340607128152));
#37265=CARTESIAN_POINT('Ctrl Pts',(-4.50601664981463,-0.230875231853538,
8.6954231047679));
#37266=CARTESIAN_POINT('Ctrl Pts',(-4.3885777553084,-4.31056627637157,7.5553097038001));
#37267=CARTESIAN_POINT('Ctrl Pts',(-4.27113886080217,-7.36800115228518,
4.62344518342595));
#37268=CARTESIAN_POINT('Ctrl Pts',(-4.15369996629594,-8.67810536521717,
0.595124871286611));
#37269=CARTESIAN_POINT('Ctrl Pts',(-4.0362610717897,-7.93018606755907,-3.57433004625461));
#37270=CARTESIAN_POINT('Ctrl Pts',(-3.91882217728347,-5.30161325262351,
-6.89612813548719));
#37271=CARTESIAN_POINT('Ctrl Pts',(-3.80138328277724,-1.41575624376498,
-8.58250083606305));
#37272=CARTESIAN_POINT('Ctrl Pts',(-3.683944388271,2.80584912651111,-8.23352275965472));
#37273=CARTESIAN_POINT('Ctrl Pts',(-3.56650549376478,6.36204387210294,-5.93195449056479));
#37274=CARTESIAN_POINT('Ctrl Pts',(-3.44906659925854,8.40947198798854,-2.2236158178687));
#37275=CARTESIAN_POINT('Ctrl Pts',(-3.33162770475231,8.46258331479401,2.01205612393598));
#37276=CARTESIAN_POINT('Ctrl Pts',(-3.21418881024607,6.50878249041422,5.77056643750267));
#37277=CARTESIAN_POINT('Ctrl Pts',(-3.09674991573985,3.01141570835078,8.16057974085834));
#37278=CARTESIAN_POINT('Ctrl Pts',(-2.97931102123361,-1.20011192280969,
8.61530134587515));
#37279=CARTESIAN_POINT('Ctrl Pts',(-2.86187212672739,-5.12703179427717,
7.0268935598338));
#37280=CARTESIAN_POINT('Ctrl Pts',(-2.74443323222114,-7.838069130789,3.77204906745287));
#37281=CARTESIAN_POINT('Ctrl Pts',(-2.62699433771492,-8.69029968045997,
-0.37734130110405));
#37282=CARTESIAN_POINT('Ctrl Pts',(-2.50955544320868,-7.48161268968305,
-4.43724523063151));
#37283=CARTESIAN_POINT('Ctrl Pts',(-2.39211654870245,-4.49865611580904,
-7.44484989363574));
#37284=CARTESIAN_POINT('Ctrl Pts',(-2.27467765419622,-0.448829370917385,
-8.68690113820128));
#37285=CARTESIAN_POINT('Ctrl Pts',(-2.15723875968999,3.70742155565816,-7.86883896867878));
#37286=CARTESIAN_POINT('Ctrl Pts',(-2.03979986518376,6.98448484914156,-5.18467964724095));
#37287=CARTESIAN_POINT('Ctrl Pts',(-1.92236097067752,8.6051058338568,-1.27095167981805));
#37288=CARTESIAN_POINT('Ctrl Pts',(-1.80492207617129,8.18513930005979,2.94415373562089));
#37289=CARTESIAN_POINT('Ctrl Pts',(-1.68748318166506,5.82381230007586,6.46110926114882));
#37290=CARTESIAN_POINT('Ctrl Pts',(-1.57004428715883,2.08184523978439,8.44568524445446));
#37291=CARTESIAN_POINT('Ctrl Pts',(-1.45260539265259,-2.15482205360423,
8.42760988040756));
#37292=CARTESIAN_POINT('Ctrl Pts',(-1.3743127963151,-4.63700526836658,7.08265443050748));
#37293=CARTESIAN_POINT('Ctrl Pts',(-1.33516649814636,-5.6465631612441,6.15675567698451));
#37294=CARTESIAN_POINT('Ctrl Pts',(-11.7398335018536,-3.76626501596132,
7.77535903219561));
#37295=CARTESIAN_POINT('Ctrl Pts',(-11.7006872036849,-5.04123441425232,
7.15778335224033));
#37296=CARTESIAN_POINT('Ctrl Pts',(-11.6223946073474,-7.2804470002415,5.28424732074805));
#37297=CARTESIAN_POINT('Ctrl Pts',(-11.5049557128412,-8.91289265768821,
1.21821348869131));
#37298=CARTESIAN_POINT('Ctrl Pts',(-11.3875168183349,-8.43150169970728,
-3.13567472513613));
#37299=CARTESIAN_POINT('Ctrl Pts',(-11.2700779238287,-5.95063940804848,
-6.74644486523312));
#37300=CARTESIAN_POINT('Ctrl Pts',(-11.1526390293225,-2.05853989085726,
-8.75702935542341));
#37301=CARTESIAN_POINT('Ctrl Pts',(-11.0352001348162,2.32172679065763,-8.69100424099601));
#37302=CARTESIAN_POINT('Ctrl Pts',(-10.91776124031,6.15140228441119,-6.56383017998038));
#37303=CARTESIAN_POINT('Ctrl Pts',(-10.8003223458038,8.5222603718995,-2.88006936326379));
#37304=CARTESIAN_POINT('Ctrl Pts',(-10.6828834512975,8.87205616180107,1.48672064508313));
#37305=CARTESIAN_POINT('Ctrl Pts',(-10.5654445567913,7.11783155898424,5.50092428542775));
#37306=CARTESIAN_POINT('Ctrl Pts',(-10.4480056622851,3.67560493837237,8.21058129693979));
#37307=CARTESIAN_POINT('Ctrl Pts',(-10.3305667677788,-0.638296289588734,
8.97308646471894));
#37308=CARTESIAN_POINT('Ctrl Pts',(-10.2131278732726,-4.80082459791572,
7.6076141283543));
#37309=CARTESIAN_POINT('Ctrl Pts',(-10.0956889787664,-7.82483144564121,
4.43798603265904));
#37310=CARTESIAN_POINT('Ctrl Pts',(-9.97825008426014,-8.99316971581067,
0.215884309006054));
#37311=CARTESIAN_POINT('Ctrl Pts',(-9.86081118975393,-8.02876659214771,
-4.05741479757908));
#37312=CARTESIAN_POINT('Ctrl Pts',(-9.74337229524768,-5.16033144692384,
-7.36849284830899));
#37313=CARTESIAN_POINT('Ctrl Pts',(-9.62593340074146,-1.06811726833064,
-8.93212366855616));
#37314=CARTESIAN_POINT('Ctrl Pts',(-9.50849450623522,3.27740225535393,-8.37749020079698));
#37315=CARTESIAN_POINT('Ctrl Pts',(-9.39105561172899,6.84568174513961,-5.8361244932828));
#37316=CARTESIAN_POINT('Ctrl Pts',(-9.27361671722275,8.79049927166384,-1.91071457815751));
#37317=CARTESIAN_POINT('Ctrl Pts',(-9.15617782271652,8.65063893182622,2.46782367969326));
#37318=CARTESIAN_POINT('Ctrl Pts',(-9.03873892821028,6.45926878019523,6.26111447528199));
#37319=CARTESIAN_POINT('Ctrl Pts',(-8.92130003370407,2.73607498108792,8.56957416337506));
#37320=CARTESIAN_POINT('Ctrl Pts',(-8.80386113919782,-1.63598241223839,
8.84574865077515));
#37321=CARTESIAN_POINT('Ctrl Pts',(-8.6864222446916,-5.62006453608818,7.02414281283443));
#37322=CARTESIAN_POINT('Ctrl Pts',(-8.56898335018536,-8.27134134570815,
3.53675274623135));
#37323=CARTESIAN_POINT('Ctrl Pts',(-8.45154445567913,-8.96105923897671,
-0.789382645310846));
#37324=CARTESIAN_POINT('Ctrl Pts',(-8.33410556117289,-7.52565075726262,
-4.92831495795738));
#37325=CARTESIAN_POINT('Ctrl Pts',(-8.21666666666667,-4.30552481228632,
-7.89849123161864));
#37326=CARTESIAN_POINT('Ctrl Pts',(-8.09922777216043,-0.0643382881177545,
-8.99553045850081));
#37327=CARTESIAN_POINT('Ctrl Pts',(-7.98178887765419,4.19210614132184,-7.95926841770293));
#37328=CARTESIAN_POINT('Ctrl Pts',(-7.86434998314797,7.45438737084802,-5.03545594464754));
#37329=CARTESIAN_POINT('Ctrl Pts',(-7.74691108864173,8.94885133807996,-0.917478813973732));
#37330=CARTESIAN_POINT('Ctrl Pts',(-7.6294721941355,8.32108404925609,3.41807956173676));
#37331=CARTESIAN_POINT('Ctrl Pts',(-7.51203329962926,5.7199612998879,6.94303610626724));
#37332=CARTESIAN_POINT('Ctrl Pts',(-7.39459440512304,1.76234259417318,8.82144297866904));
#37333=CARTESIAN_POINT('Ctrl Pts',(-7.27715551061681,-2.61321785578727,
8.60783364635613));
#37334=CARTESIAN_POINT('Ctrl Pts',(-7.15971661611056,-6.36905043197742,
6.35286582890546));
#37335=CARTESIAN_POINT('Ctrl Pts',(-7.04227772160434,-8.61445475458585,
2.59130795667739));
#37336=CARTESIAN_POINT('Ctrl Pts',(-6.92483882709811,-8.81693038798178,
-1.78478182942051));
#37337=CARTESIAN_POINT('Ctrl Pts',(-6.80739993259187,-6.92845998317274,
-5.73760837864699));
#37338=CARTESIAN_POINT('Ctrl Pts',(-6.68996103808565,-3.3968966520065,-8.32975394478933));
#37339=CARTESIAN_POINT('Ctrl Pts',(-6.5725221435794,0.940244956877155,-8.94648797384835));
#37340=CARTESIAN_POINT('Ctrl Pts',(-6.45508324907318,5.05440630154049,-7.44155122162673));
#37341=CARTESIAN_POINT('Ctrl Pts',(-6.33764435456694,7.96990888781211,-4.17184131590833));
#37342=CARTESIAN_POINT('Ctrl Pts',(-6.22020546006072,8.99533764107029,0.0872259611020821));
#37343=CARTESIAN_POINT('Ctrl Pts',(-6.10276656555447,7.88751085353959,4.32560749264671));
#37344=CARTESIAN_POINT('Ctrl Pts',(-5.98532767104826,4.90915102959206,7.53816581230484));
#37345=CARTESIAN_POINT('Ctrl Pts',(-5.86788877654201,0.766579916161399,
8.96303870778679));
#37346=CARTESIAN_POINT('Ctrl Pts',(-5.75044988203579,-3.55778658048453,
8.26231579479207));
#37347=CARTESIAN_POINT('Ctrl Pts',(-5.63301098752954,-7.03841955220852,
5.60217438609644));
#37348=CARTESIAN_POINT('Ctrl Pts',(-5.51557209302333,-8.84988254863418,
1.61347033456665));
#37349=CARTESIAN_POINT('Ctrl Pts',(-5.39813319851708,-8.56258486085733,
-2.757870219166));
#37350=CARTESIAN_POINT('Ctrl Pts',(-5.28069430401086,-6.24465949385924,
-6.47517841073899));
#37351=CARTESIAN_POINT('Ctrl Pts',(-5.16325540950462,-2.44580533939745,
-8.65688996620155));
#37352=CARTESIAN_POINT('Ctrl Pts',(-5.04581651499839,1.93307460177137,-8.78560926909064));
#37353=CARTESIAN_POINT('Ctrl Pts',(-4.92837762049216,5.85352349015212,-6.83081037618444));
#37354=CARTESIAN_POINT('Ctrl Pts',(-4.81093872598592,8.38580198218156,-3.25607628300896));
#37355=CARTESIAN_POINT('Ctrl Pts',(-4.69349983147969,8.92937707515854,1.0908403617408));
#37356=CARTESIAN_POINT('Ctrl Pts',(-4.57606093697346,7.35533925781453,5.17906285418186));
#37357=CARTESIAN_POINT('Ctrl Pts',(-4.45862204246723,4.0369735617288,8.03906413129479));
#37358=CARTESIAN_POINT('Ctrl Pts',(-4.34118314796099,-0.238765449556927,
8.99259132315565));
#37359=CARTESIAN_POINT('Ctrl Pts',(-4.22374425345476,-4.45788093664258,
7.81351426693571));
#37360=CARTESIAN_POINT('Ctrl Pts',(-4.10630535894853,-7.61980439970885,
4.78145255712337));
#37361=CARTESIAN_POINT('Ctrl Pts',(-3.98886646444229,-8.97468174560615,
0.615463409801377));
#37362=CARTESIAN_POINT('Ctrl Pts',(-3.87142756993607,-8.20120212241758,
-3.69648365269531));
#37363=CARTESIAN_POINT('Ctrl Pts',(-3.75398867542983,-5.48279718650238,
-7.1318050067682));
#37364=CARTESIAN_POINT('Ctrl Pts',(-3.6365497809236,-1.46414006081009,-8.87580990820765));
#37365=CARTESIAN_POINT('Ctrl Pts',(-3.51911088641737,2.90173970894095,-8.51490542040183));
#37366=CARTESIAN_POINT('Ctrl Pts',(-3.40167199191113,6.57946828262311,-6.13468049093065));
#37367=CARTESIAN_POINT('Ctrl Pts',(-3.28423309740491,8.69686775679039,-2.29960843410063));
#37368=CARTESIAN_POINT('Ctrl Pts',(-3.16679420289867,8.7517941762225,2.0808186357128));
#37369=CARTESIAN_POINT('Ctrl Pts',(-3.04935530839244,6.73122172922358,5.96777696155187));
#37370=CARTESIAN_POINT('Ctrl Pts',(-2.93191641388621,3.11433157915927,8.43946955603849));
#37371=CARTESIAN_POINT('Ctrl Pts',(-2.81447751937998,-1.24112604226888,
8.90973138349155));
#37372=CARTESIAN_POINT('Ctrl Pts',(-2.69703862487374,-5.30224936397625,
7.26703937158057));
#37373=CARTESIAN_POINT('Ctrl Pts',(-2.57959973036751,-8.1059370667287,3.9009597699616));
#37374=CARTESIAN_POINT('Ctrl Pts',(-2.46216083586128,-8.98729280456475,
-0.390237032665602));
#37375=CARTESIAN_POINT('Ctrl Pts',(-2.34472194135504,-7.7372986392766,-4.58888917525028));
#37376=CARTESIAN_POINT('Ctrl Pts',(-2.22728304684881,-4.65239879249847,
-7.69927946565311));
#37377=CARTESIAN_POINT('Ctrl Pts',(-2.10984415234258,-0.46416822480737,
-8.98377811629039));
#37378=CARTESIAN_POINT('Ctrl Pts',(-1.99240525783635,3.83412359709224,-8.13775847137902));
#37379=CARTESIAN_POINT('Ctrl Pts',(-1.87496636333012,7.22318133279369,-5.36186734646136));
#37380=CARTESIAN_POINT('Ctrl Pts',(-1.75752746882388,8.89918743734806,-1.31438676535649));
#37381=CARTESIAN_POINT('Ctrl Pts',(-1.64008857431765,8.46486844420237,3.04477091200582));
#37382=CARTESIAN_POINT('Ctrl Pts',(-1.52264967981142,6.02284251454457,6.68191925564942));
#37383=CARTESIAN_POINT('Ctrl Pts',(-1.40521078530519,2.15299281172101,8.73431861018245));
#37384=CARTESIAN_POINT('Ctrl Pts',(-1.28777189079896,-2.22846362606102,
8.71562551613373));
#37385=CARTESIAN_POINT('Ctrl Pts',(-1.20947929446147,-4.79547606129435,
7.32470588369278));
#37386=CARTESIAN_POINT('Ctrl Pts',(-1.17033299629272,-5.83953584289782,
6.36716431306054));
#37387=CARTESIAN_POINT('Ctrl Pts',(-11.575,-3.8907246099259,8.03230272149382));
#37388=CARTESIAN_POINT('Ctrl Pts',(-11.5358537018313,-5.20782651162705,
7.39431870116847));
#37389=CARTESIAN_POINT('Ctrl Pts',(-11.4575611054938,-7.52103587906191,
5.45886999683736));
#37390=CARTESIAN_POINT('Ctrl Pts',(-11.3401222109875,-9.20742716243616,
1.25847044233695));
#37391=CARTESIAN_POINT('Ctrl Pts',(-11.2226833164813,-8.71012820995283,
-3.2392958992812));
#37392=CARTESIAN_POINT('Ctrl Pts',(-11.1052444219751,-6.14728360632359,
-6.96938716617923));
#37393=CARTESIAN_POINT('Ctrl Pts',(-10.9878055274688,-2.12656618159628,
-9.04641321802813));
#37394=CARTESIAN_POINT('Ctrl Pts',(-10.8703666329626,2.39845032775268,-8.97820624467727));
#37395=CARTESIAN_POINT('Ctrl Pts',(-10.7529277384564,6.35468087138952,-6.78073781542045));
#37396=CARTESIAN_POINT('Ctrl Pts',(-10.6354888439501,8.80388608359315,-2.97524382975048));
#37397=CARTESIAN_POINT('Ctrl Pts',(-10.5180499494439,9.16524118804035,1.53585065771941));
#37398=CARTESIAN_POINT('Ctrl Pts',(-10.4006110549377,7.35304666519293,5.68270724549368));
#37399=CARTESIAN_POINT('Ctrl Pts',(-10.2831721604314,3.79706858903565,8.48190729500407));
#37400=CARTESIAN_POINT('Ctrl Pts',(-10.1657332659252,-0.659389361025453,
9.26961012762504));
#37401=CARTESIAN_POINT('Ctrl Pts',(-10.048294371419,-4.95947213801698,7.85901453736469));
#37402=CARTESIAN_POINT('Ctrl Pts',(-9.93085547691273,-8.08340999506311,
4.58464324804467));
#37403=CARTESIAN_POINT('Ctrl Pts',(-9.81341658240652,-9.2903570477007,0.22301839896743));
#37404=CARTESIAN_POINT('Ctrl Pts',(-9.69597768790027,-8.29408436077532,
-4.19149569632424));
#37405=CARTESIAN_POINT('Ctrl Pts',(-9.57853879339405,-5.33085921219923,
-7.61199128087941));
#37406=CARTESIAN_POINT('Ctrl Pts',(-9.4610998988878,-1.10341415820951,-9.22729367924807));
#37407=CARTESIAN_POINT('Ctrl Pts',(-9.34366100438159,3.38570694241956,-8.65433185278234));
#37408=CARTESIAN_POINT('Ctrl Pts',(-9.22622210987534,7.07190341748608,-6.02898444383924));
#37409=CARTESIAN_POINT('Ctrl Pts',(-9.10878321536913,9.08098917756812,-1.9738558493033));
#37410=CARTESIAN_POINT('Ctrl Pts',(-8.99134432086287,8.93650702778507,2.5493751190766));
#37411=CARTESIAN_POINT('Ctrl Pts',(-8.87390542635666,6.67272109071619,6.46801859967495));
#37412=CARTESIAN_POINT('Ctrl Pts',(-8.75646653185042,2.82649102450486,8.8527634015999));
#37413=CARTESIAN_POINT('Ctrl Pts',(-8.63902763734418,-1.69004491338938,
9.13806432179736));
#37414=CARTESIAN_POINT('Ctrl Pts',(-8.52158874283796,-5.80578459223184,
7.25626189068202));
#37415=CARTESIAN_POINT('Ctrl Pts',(-8.40414984833171,-8.54467521389493,
3.65362790209096));
#37416=CARTESIAN_POINT('Ctrl Pts',(-8.28671095382549,-9.25718545145751,
-0.815468500422392));
#37417=CARTESIAN_POINT('Ctrl Pts',(-8.16927205931925,-7.77434261341153,
-5.09117553096471));
#37418=CARTESIAN_POINT('Ctrl Pts',(-8.05183316481303,-4.447804728243,-8.15950393450966));
#37419=CARTESIAN_POINT('Ctrl Pts',(-7.93439427030679,-0.0664644043580101,
-9.29279580324321));
#37420=CARTESIAN_POINT('Ctrl Pts',(-7.81695537580056,4.33063803591613,-8.22228955703439));
#37421=CARTESIAN_POINT('Ctrl Pts',(-7.69951648129433,7.70072426469339,-5.20185708732905));
#37422=CARTESIAN_POINT('Ctrl Pts',(-7.58207758678809,9.24457412956349,-0.947797721478743));
#37423=CARTESIAN_POINT('Ctrl Pts',(-7.46463869228187,8.59606170954461,3.53103305613757));
#37424=CARTESIAN_POINT('Ctrl Pts',(-7.34719979777562,5.90898253388501,7.1724749404983));
#37425=CARTESIAN_POINT('Ctrl Pts',(-7.2297609032694,1.82058078048448,9.11295544703064));
#37426=CARTESIAN_POINT('Ctrl Pts',(-7.11232200876316,-2.69957397568162,
8.8922872033947));
#37427=CARTESIAN_POINT('Ctrl Pts',(-6.99488311425694,-6.57952139653898,
6.56280195879174));
#37428=CARTESIAN_POINT('Ctrl Pts',(-6.8774442197507,-8.89912711206419,2.67694004437129));
#37429=CARTESIAN_POINT('Ctrl Pts',(-6.76000532524447,-9.10829373375051,
-1.84376154031808));
#37430=CARTESIAN_POINT('Ctrl Pts',(-6.64256643073823,-7.15741713638714,
-5.9272127761357));
#37431=CARTESIAN_POINT('Ctrl Pts',(-6.52512753623201,-3.50915013822074,
-8.60501810952541));
#37432=CARTESIAN_POINT('Ctrl Pts',(-6.40768864172577,0.971316191924136,
-9.24213266584832));
#37433=CARTESIAN_POINT('Ctrl Pts',(-6.29024974721955,5.22143367570448,-7.68746393344737));
#37434=CARTESIAN_POINT('Ctrl Pts',(-6.1728108527133,8.23328165098941,-4.30970354123293));
#37435=CARTESIAN_POINT('Ctrl Pts',(-6.05537195820708,9.29259661398837,0.0901084209544563));
#37436=CARTESIAN_POINT('Ctrl Pts',(-5.93793306370083,8.14816070002208,4.468551058727));
#37437=CARTESIAN_POINT('Ctrl Pts',(-5.82049416919461,5.07137831345671,7.78727123963432));
#37438=CARTESIAN_POINT('Ctrl Pts',(-5.70305527468838,0.791912234705773,
9.25923033358377));
#37439=CARTESIAN_POINT('Ctrl Pts',(-5.58561638018215,-3.67535681819832,
8.53535140558126));
#37440=CARTESIAN_POINT('Ctrl Pts',(-5.46817748567591,-7.27101041767012,
5.78730324624234));
#37441=CARTESIAN_POINT('Ctrl Pts',(-5.35073859116969,-9.14233482800627,
1.66678890398835));
#37442=CARTESIAN_POINT('Ctrl Pts',(-5.23329969666344,-8.84554313133302,
-2.8490065057071));
#37443=CARTESIAN_POINT('Ctrl Pts',(-5.11586080215722,-6.45101984868266,
-6.68915646922223));
#37444=CARTESIAN_POINT('Ctrl Pts',(-4.99842190765098,-2.52662916304442,
-8.94296463317886));
#37445=CARTESIAN_POINT('Ctrl Pts',(-4.88098301314475,1.99695477988418,-9.07593758048892));
#37446=CARTESIAN_POINT('Ctrl Pts',(-4.76354411863852,6.04695840611235,-7.05654061085087));
#37447=CARTESIAN_POINT('Ctrl Pts',(-4.64610522413228,8.66291830441234,-3.36367623425603));
#37448=CARTESIAN_POINT('Ctrl Pts',(-4.52866632962606,9.22445632221657,1.12688815655265));
#37449=CARTESIAN_POINT('Ctrl Pts',(-4.41122743511982,7.5984030182296,5.35020961555334));
#37450=CARTESIAN_POINT('Ctrl Pts',(-4.29378854061359,4.1703789615637,8.30472219130806));
#37451=CARTESIAN_POINT('Ctrl Pts',(-4.17634964610736,-0.246655667260323,
9.28975954154339));
#37452=CARTESIAN_POINT('Ctrl Pts',(-4.05891075160113,-4.60519559691359,
8.07171883007134));
#37453=CARTESIAN_POINT('Ctrl Pts',(-3.94147185709489,-7.87160764713254,
4.93945993082077));
#37454=CARTESIAN_POINT('Ctrl Pts',(-3.82403296258866,-9.27125812599511,
0.635801948316151));
#37455=CARTESIAN_POINT('Ctrl Pts',(-3.70659406808243,-8.47221817727612,
-3.81863725913602));
#37456=CARTESIAN_POINT('Ctrl Pts',(-3.5891551735762,-5.66398112038124,-7.36748187804921));
#37457=CARTESIAN_POINT('Ctrl Pts',(-3.47171627906996,-1.51252387785522,
-9.16911898035225));
#37458=CARTESIAN_POINT('Ctrl Pts',(-3.35427738456373,2.99763029137079,-8.79628808114895));
#37459=CARTESIAN_POINT('Ctrl Pts',(-3.23683849005749,6.79689269314325,-6.3374064912965));
#37460=CARTESIAN_POINT('Ctrl Pts',(-3.11939959555127,8.98426352559225,-2.37560105033256));
#37461=CARTESIAN_POINT('Ctrl Pts',(-3.00196070104503,9.041005037651,2.14958114748964));
#37462=CARTESIAN_POINT('Ctrl Pts',(-2.8845218065388,6.95366096803292,6.16498748560106));
#37463=CARTESIAN_POINT('Ctrl Pts',(-2.76708291203257,3.21724744996777,8.71835937121864));
#37464=CARTESIAN_POINT('Ctrl Pts',(-2.64964401752634,-1.28214016172808,
9.20416142110794));
#37465=CARTESIAN_POINT('Ctrl Pts',(-2.5322051230201,-5.47746693367532,7.50718518332735));
#37466=CARTESIAN_POINT('Ctrl Pts',(-2.41476622851387,-8.3738050026684,4.02987047247031));
#37467=CARTESIAN_POINT('Ctrl Pts',(-2.29732733400764,-9.28428592866953,
-0.403132764227142));
#37468=CARTESIAN_POINT('Ctrl Pts',(-2.17988843950141,-7.99298458887015,
-4.74053311986907));
#37469=CARTESIAN_POINT('Ctrl Pts',(-2.06244954499517,-4.8061414691879,-7.95370903767045));
#37470=CARTESIAN_POINT('Ctrl Pts',(-1.94501065048894,-0.479507078697361,
-9.28065509437951));
#37471=CARTESIAN_POINT('Ctrl Pts',(-1.82757175598271,3.96082563852633,-8.40667797407926));
#37472=CARTESIAN_POINT('Ctrl Pts',(-1.71013286147648,7.46187781644582,-5.53905504568178));
#37473=CARTESIAN_POINT('Ctrl Pts',(-1.59269396697024,9.19326904083934,-1.35782185089492));
#37474=CARTESIAN_POINT('Ctrl Pts',(-1.47525507246401,8.74459758834494,3.14538808839074));
#37475=CARTESIAN_POINT('Ctrl Pts',(-1.35781617795778,6.2218727290133,6.90272925015002));
#37476=CARTESIAN_POINT('Ctrl Pts',(-1.24037728345155,2.22414038365762,9.02295197591045));
#37477=CARTESIAN_POINT('Ctrl Pts',(-1.12293838894532,-2.3021051985178,9.0036411518599));
#37478=CARTESIAN_POINT('Ctrl Pts',(-1.04464579260783,-4.95394685422212,
7.56675733687807));
#37479=CARTESIAN_POINT('Ctrl Pts',(-1.00549949443908,-6.03250852455154,
6.57757294913656));
#37480=CARTESIAN_POINT('',(-1.5,8.66570476755281,2.13569330232889));
#37481=CARTESIAN_POINT('Ctrl Pts',(-1.5,8.66576000559871,2.13591603404143));
#37482=CARTESIAN_POINT('Ctrl Pts',(-1.5,8.60143786733659,2.35388806264619));
#37483=CARTESIAN_POINT('Ctrl Pts',(-1.5,8.52891377544564,2.56895211712534));
#37484=CARTESIAN_POINT('Ctrl Pts',(-1.5,8.4482767600922,2.78063200867923));
#37485=CARTESIAN_POINT('Ctrl Pts',(-1.5,8.41941943948704,2.85638524023751));
#37486=CARTESIAN_POINT('Ctrl Pts',(-1.5,8.38952263531352,2.93170495461832));
#37487=CARTESIAN_POINT('Ctrl Pts',(-1.5,8.3585888708654,3.00656886656796));
#37488=CARTESIAN_POINT('Ctrl Pts',(-1.5,8.27217290574518,3.2157072407433));
#37489=CARTESIAN_POINT('Ctrl Pts',(-1.5,8.17766782067611,3.42129027050491));
#37490=CARTESIAN_POINT('Ctrl Pts',(-1.5,8.07540183938106,3.62292678990022));
#37491=CARTESIAN_POINT('Ctrl Pts',(-1.5,7.97289129821306,3.82504550485008));
#37492=CARTESIAN_POINT('Ctrl Pts',(-1.5,7.86258227404303,4.0231993593376));
#37493=CARTESIAN_POINT('Ctrl Pts',(-1.5,7.74476169665056,4.216965576945));
#37494=CARTESIAN_POINT('Ctrl Pts',(-1.5,7.62760726374108,4.40963626183896));
#37495=CARTESIAN_POINT('Ctrl Pts',(-1.5,7.50302551968923,4.59796928062881));
#37496=CARTESIAN_POINT('Ctrl Pts',(-1.5,7.37126210654191,4.78151280564942));
#37497=CARTESIAN_POINT('Ctrl Pts',(-1.5,7.31559889864895,4.85905042513419));
#37498=CARTESIAN_POINT('Ctrl Pts',(-1.5,7.25865362523378,4.93573281300596));
#37499=CARTESIAN_POINT('Ctrl Pts',(-1.5,7.20044313369025,5.01152361846556));
#37500=CARTESIAN_POINT('Ctrl Pts',(-1.5,7.16709059230978,5.05494905447067));
#37501=CARTESIAN_POINT('Ctrl Pts',(-1.5,7.13332267751954,5.09808176810313));
#37502=CARTESIAN_POINT('Ctrl Pts',(-1.5,7.09914242712044,5.14091470044488));
#37503=CARTESIAN_POINT('Ctrl Pts',(-1.5,7.08237376420541,5.16192832660953));
#37504=CARTESIAN_POINT('Ctrl Pts',(-1.5,7.06550518246979,5.18287056042006));
#37505=CARTESIAN_POINT('Ctrl Pts',(-1.5,7.04854790718269,5.20372738131514));
#37506=CARTESIAN_POINT('Ctrl Pts',(-1.5,6.90705671288669,5.3777563127147));
#37507=CARTESIAN_POINT('Ctrl Pts',(-1.5,6.75922259168711,5.54605767871865));
#37508=CARTESIAN_POINT('Ctrl Pts',(-1.5,6.60536289902919,5.70825802077741));
#37509=CARTESIAN_POINT('Ctrl Pts',(-1.5,6.45204887458798,5.86988311424524));
#37510=CARTESIAN_POINT('Ctrl Pts',(-1.5,6.29275147947152,6.02545086754665));
#37511=CARTESIAN_POINT('Ctrl Pts',(-1.5,6.12774643390987,6.17455745002506));
#37512=CARTESIAN_POINT('Ctrl Pts',(-1.5,6.02442900763097,6.26792010018206));
#37513=CARTESIAN_POINT('Ctrl Pts',(-1.5,5.91887310495571,6.35874887481627));
#37514=CARTESIAN_POINT('Ctrl Pts',(-1.5,5.81113993546571,6.44693645990187));
#37515=CARTESIAN_POINT('Ctrl Pts',(-1.5,5.6382749924561,6.58843922958872));
#37516=CARTESIAN_POINT('Ctrl Pts',(-1.5,5.45980530418602,6.72314435409563));
#37517=CARTESIAN_POINT('Ctrl Pts',(-1.5,5.27618003291779,6.85081401922972));
#37518=CARTESIAN_POINT('Ctrl Pts',(-1.5,5.0936053673245,6.97775322676513));
#37519=CARTESIAN_POINT('Ctrl Pts',(-1.5,4.90593330226794,7.09773747877284));
#37520=CARTESIAN_POINT('Ctrl Pts',(-1.5,4.71358884520666,7.21048451846429));
#37521=CARTESIAN_POINT('Ctrl Pts',(-1.5,4.65195078987431,7.24661505415655));
#37522=CARTESIAN_POINT('Ctrl Pts',(-1.5,4.58983282761987,7.28200199438233));
#37523=CARTESIAN_POINT('Ctrl Pts',(-1.5,4.52724874890727,7.31663492807838));
#37524=CARTESIAN_POINT('Ctrl Pts',(-1.5,4.50584961293089,7.32847683536004));
#37525=CARTESIAN_POINT('Ctrl Pts',(-1.5,4.48439782036337,7.34022953024155));
#37526=CARTESIAN_POINT('Ctrl Pts',(-1.5,4.46290386332694,7.35188735834325));
#37527=CARTESIAN_POINT('Ctrl Pts',(-1.5,4.2684954791601,7.45732999602529));
#37528=CARTESIAN_POINT('Ctrl Pts',(-1.5,4.07041460477949,7.55514065186345));
#37529=CARTESIAN_POINT('Ctrl Pts',(-1.5,3.86912729317476,7.64515288152635));
#37530=CARTESIAN_POINT('Ctrl Pts',(-1.5,3.66778053053916,7.73519169666949));
#37531=CARTESIAN_POINT('Ctrl Pts',(-1.5,3.46322479181838,7.81742772613441));
#37532=CARTESIAN_POINT('Ctrl Pts',(-1.5,3.25590400874615,7.8916473356843));
#37533=CARTESIAN_POINT('Ctrl Pts',(-1.5,3.050998079672,7.96500244183901));
#37534=CARTESIAN_POINT('Ctrl Pts',(-1.5,2.84339051416899,8.03052693585015));
#37535=CARTESIAN_POINT('Ctrl Pts',(-1.5,2.63349743742722,8.08796583453746));
#37536=CARTESIAN_POINT('Ctrl Pts',(-1.5,2.43376039741608,8.14262545353679));
#37537=CARTESIAN_POINT('Ctrl Pts',(-1.5,2.23195315073253,8.18996285358873));
#37538=CARTESIAN_POINT('Ctrl Pts',(-1.5,2.02843125000073,8.22971455260885));
#37539=CARTESIAN_POINT('Ctrl Pts',(-1.5,1.85980622697303,8.26265022753403));
#37540=CARTESIAN_POINT('Ctrl Pts',(-1.5,1.69000390546641,8.29037758188515));
#37541=CARTESIAN_POINT('Ctrl Pts',(-1.5,1.51926769823031,8.31287539192494));
#37542=CARTESIAN_POINT('Ctrl Pts',(-1.5,1.48148098969113,8.31785452438024));
#37543=CARTESIAN_POINT('Ctrl Pts',(-1.5,1.44364855517463,8.32257743549686));
#37544=CARTESIAN_POINT('Ctrl Pts',(-1.5,1.40577306551694,8.32704377013679));
#37545=CARTESIAN_POINT('Ctrl Pts',(-1.5,1.37905825216086,8.3301940210608));
#37546=CARTESIAN_POINT('Ctrl Pts',(-1.5,1.35232071229212,8.3332167220265));
#37547=CARTESIAN_POINT('Ctrl Pts',(-1.5,1.32557926688546,8.33610993612108));
#37548=CARTESIAN_POINT('Ctrl Pts',(-1.5,1.11025704115137,8.35940610762172));
#37549=CARTESIAN_POINT('Ctrl Pts',(-1.5,0.894419768746766,8.37434346908902));
#37550=CARTESIAN_POINT('Ctrl Pts',(-1.5,0.67855625163336,8.38101089356783));
#37551=CARTESIAN_POINT('Ctrl Pts',(-1.5,0.461134916361629,8.38772643472268));
#37552=CARTESIAN_POINT('Ctrl Pts',(-1.5,0.243686264614475,8.38605221878385));
#37553=CARTESIAN_POINT('Ctrl Pts',(-1.5,0.0267066921148425,8.37602648219115));
#37554=CARTESIAN_POINT('Ctrl Pts',(-1.5,-0.18935948302369,8.36604294994628));
#37555=CARTESIAN_POINT('Ctrl Pts',(-1.5,-0.404961196433814,8.34777795012559));
#37556=CARTESIAN_POINT('Ctrl Pts',(-1.5,-0.619601062333341,8.32121848102122));
#37557=CARTESIAN_POINT('Ctrl Pts',(-1.5,-0.832145718967339,8.29491827244855));
#37558=CARTESIAN_POINT('Ctrl Pts',(-1.5,-1.04374783796762,8.26048459624622));
#37559=CARTESIAN_POINT('Ctrl Pts',(-1.5,-1.25390771612789,8.21785690077272));
#37560=CARTESIAN_POINT('Ctrl Pts',(-1.5,-1.38779584224784,8.19069975585181));
#37561=CARTESIAN_POINT('Ctrl Pts',(-1.5,-1.52109824477793,8.16021596832127));
#37562=CARTESIAN_POINT('Ctrl Pts',(-1.5,-1.6536803677507,8.12637995005445));
#37563=CARTESIAN_POINT('Ctrl Pts',(-1.5,-1.71355702926136,8.11109894710169));
#37564=CARTESIAN_POINT('Ctrl Pts',(-1.5,-1.77328671763606,8.09513411894022));
#37565=CARTESIAN_POINT('Ctrl Pts',(-1.5,-1.8328566920054,8.07848259714385));
#37566=CARTESIAN_POINT('Ctrl Pts',(-1.5,-1.85625104511745,8.07194320234166));
#37567=CARTESIAN_POINT('Ctrl Pts',(-1.5,-1.87961849607907,8.06529850226245));
#37568=CARTESIAN_POINT('Ctrl Pts',(-1.5,-1.90294990325727,8.05855087488496));
#37569=CARTESIAN_POINT('Ctrl Pts',(-1.5,-1.95175693881833,8.04443549440875));
#37570=CARTESIAN_POINT('Ctrl Pts',(-1.5,-2.0004168594957,8.02986675849686));
#37571=CARTESIAN_POINT('Ctrl Pts',(-1.5,-2.04892326796492,8.01484480928137));
#37572=CARTESIAN_POINT('Ctrl Pts',(-1.5,-2.25391562363821,7.95136072844197));
#37573=CARTESIAN_POINT('Ctrl Pts',(-1.5,-2.45616780304103,7.87978621926163));
#37574=CARTESIAN_POINT('Ctrl Pts',(-1.5,-2.65527234953228,7.80041100969696));
#37575=CARTESIAN_POINT('Ctrl Pts',(-1.5,-2.85500999528719,7.72078340817231));
#37576=CARTESIAN_POINT('Ctrl Pts',(-1.5,-3.05158055128827,7.63330504161439));
#37577=CARTESIAN_POINT('Ctrl Pts',(-1.5,-3.24454813151519,7.53822212811181));
#37578=CARTESIAN_POINT('Ctrl Pts',(-1.5,-3.34675198073698,7.48786216741915));
#37579=CARTESIAN_POINT('Ctrl Pts',(-1.5,-3.44794465250143,7.43536822680612));
#37580=CARTESIAN_POINT('Ctrl Pts',(-1.5,-3.54805774165375,7.38077220333937));
#37581=CARTESIAN_POINT('Ctrl Pts',(-1.5,-3.62664687830836,7.33791412768357));
#37582=CARTESIAN_POINT('Ctrl Pts',(-1.5,-3.70457069537403,7.29376061887687));
#37583=CARTESIAN_POINT('Ctrl Pts',(-1.5,-3.78179482379092,7.24832583256977));
#37584=CARTESIAN_POINT('Ctrl Pts',(-1.5,-3.80711424857812,7.23342915871656));
#37585=CARTESIAN_POINT('Ctrl Pts',(-1.5,-3.83235671992797,7.218395710483));
#37586=CARTESIAN_POINT('Ctrl Pts',(-1.5,-3.85751122859775,7.2032320690579));
#37587=CARTESIAN_POINT('Ctrl Pts',(-1.5,-4.04011948514428,7.09315215615307));
#37588=CARTESIAN_POINT('Ctrl Pts',(-1.5,-4.21824071284525,6.97612901123971));
#37589=CARTESIAN_POINT('Ctrl Pts',(-1.5,-4.39146092341165,6.85242058055038));
#37590=CARTESIAN_POINT('Ctrl Pts',(-1.5,-4.56386961582583,6.72929171062224));
#37591=CARTESIAN_POINT('Ctrl Pts',(-1.5,-4.73142363312739,6.59953962500907));
#37592=CARTESIAN_POINT('Ctrl Pts',(-1.5,-4.89368134090825,6.46337959276038));
#37593=CARTESIAN_POINT('Ctrl Pts',(-1.5,-5.05352274842095,6.32924722087332));
#37594=CARTESIAN_POINT('Ctrl Pts',(-1.5,-5.20822483934881,6.18889589430103));
#37595=CARTESIAN_POINT('Ctrl Pts',(-1.5,-5.35732594311023,6.04249986337617));
#37596=CARTESIAN_POINT('Ctrl Pts',(-1.5,-5.38967967618284,6.01073310922114));
#37597=CARTESIAN_POINT('Ctrl Pts',(-1.5,-5.42176952083074,5.97868163150745));
#37598=CARTESIAN_POINT('Ctrl Pts',(-1.5,-5.45359047959038,5.94634704090849));
#37599=CARTESIAN_POINT('Ctrl Pts',(-2.3076868253652,-8.92557695889132,-0.000120900814251108));
#37600=CARTESIAN_POINT('Ctrl Pts',(-2.30423366157935,-8.92566437048567,
-0.129190724569353));
#37601=CARTESIAN_POINT('Ctrl Pts',(-2.30078049779349,-8.92292102407511,
-0.258256830648859));
#37602=CARTESIAN_POINT('Ctrl Pts',(-2.29732733400764,-8.91732221770278,
-0.387198950717887));
#37603=CARTESIAN_POINT('Ctrl Pts',(-2.2581810358389,-8.8538521487364,-1.84893288277443));
#37604=CARTESIAN_POINT('Ctrl Pts',(-2.21903473767015,-8.42341836880329,
-3.29473300132172));
#37605=CARTESIAN_POINT('Ctrl Pts',(-2.17988843950141,-7.6770609588897,-4.55316238022893));
#37606=CARTESIAN_POINT('Ctrl Pts',(-2.14074214133266,-6.93070354897609,
-5.81159175913617));
#37607=CARTESIAN_POINT('Ctrl Pts',(-2.10159584316392,-5.868422509082,-6.88265039840332));
#37608=CARTESIAN_POINT('Ctrl Pts',(-2.06244954499517,-4.6161762573865,-7.63933739415508));
#37609=CARTESIAN_POINT('Ctrl Pts',(-2.02330324682643,-3.36393000569105,
-8.39602438990681));
#37610=CARTESIAN_POINT('Ctrl Pts',(-1.98415694865769,-1.92171854219422,
-8.83833974214316));
#37611=CARTESIAN_POINT('Ctrl Pts',(-1.94501065048894,-0.46055735757519,
-8.91383456487796));
#37612=CARTESIAN_POINT('Ctrl Pts',(-1.9058643523202,1.00060382704386,-8.98932938761276));
#37613=CARTESIAN_POINT('Ctrl Pts',(-1.86671805415145,2.48071473278515,-8.698003680846));
#37614=CARTESIAN_POINT('Ctrl Pts',(-1.82757175598271,3.80427888197568,-8.07440367272969));
#37615=CARTESIAN_POINT('Ctrl Pts',(-1.78842545781396,5.1278430311662,-7.4508036646134));
#37616=CARTESIAN_POINT('Ctrl Pts',(-1.74927915964522,6.294860423806,-6.49492935514759));
#37617=CARTESIAN_POINT('Ctrl Pts',(-1.71013286147648,7.16693432419149,-5.32012000128355));
#37618=CARTESIAN_POINT('Ctrl Pts',(-1.67098656330773,8.03900822457701,-4.14531064741947));
#37619=CARTESIAN_POINT('Ctrl Pts',(-1.63184026513899,8.61613863270816,-2.75156624915723));
#37620=CARTESIAN_POINT('Ctrl Pts',(-1.59269396697024,8.82992526135802,-1.30415906014512));
#37621=CARTESIAN_POINT('Ctrl Pts',(-1.56179597798016,8.99866604164268,-0.161727374842938));
#37622=CARTESIAN_POINT('Ctrl Pts',(-1.53089798899008,8.94104834757229,1.01413553490768));
#37623=CARTESIAN_POINT('Ctrl Pts',(-1.5,8.66576000559871,2.13591603404143));
#37624=CARTESIAN_POINT('',(-11.575,-4.68253987355576,-6.57073151046064));
#37625=CARTESIAN_POINT('Ctrl Pts',(-11.575,-4.68274545894496,-6.57070370794207));
#37626=CARTESIAN_POINT('Ctrl Pts',(-11.575,-4.862640076186,-6.45616650491057));
#37627=CARTESIAN_POINT('Ctrl Pts',(-11.575,-5.03774328114105,-6.33464824857975));
#37628=CARTESIAN_POINT('Ctrl Pts',(-11.575,-5.20761491997005,-6.20640283237483));
#37629=CARTESIAN_POINT('Ctrl Pts',(-11.575,-5.26094487773974,-6.16614112254786));
#37630=CARTESIAN_POINT('Ctrl Pts',(-11.575,-5.31375908988843,-6.12521601726515));
#37631=CARTESIAN_POINT('Ctrl Pts',(-11.575,-5.36604355027271,-6.08363438702985));
#37632=CARTESIAN_POINT('Ctrl Pts',(-11.575,-5.53158882597289,-5.95197686602315));
#37633=CARTESIAN_POINT('Ctrl Pts',(-11.575,-5.69182547913848,-5.81374097888015));
#37634=CARTESIAN_POINT('Ctrl Pts',(-11.575,-5.84650148035433,-5.66935359056696));
#37635=CARTESIAN_POINT('Ctrl Pts',(-11.575,-5.95031524401272,-5.57244522671108));
#37636=CARTESIAN_POINT('Ctrl Pts',(-11.575,-6.05162357167362,-5.47276482909323));
#37637=CARTESIAN_POINT('Ctrl Pts',(-11.575,-6.1503422410466,-5.37043108239685));
#37638=CARTESIAN_POINT('Ctrl Pts',(-11.575,-6.18235090099834,-5.33725026543085));
#37639=CARTESIAN_POINT('Ctrl Pts',(-11.575,-6.21408724871341,-5.30379043579792));
#37640=CARTESIAN_POINT('Ctrl Pts',(-11.575,-6.24554824847592,-5.27005547302152));
#37641=CARTESIAN_POINT('Ctrl Pts',(-11.575,-6.27435701813293,-5.23916444033503));
#37642=CARTESIAN_POINT('Ctrl Pts',(-11.575,-6.30293851147707,-5.20803860034052));
#37643=CARTESIAN_POINT('Ctrl Pts',(-11.575,-6.33126902715642,-5.17670480194982));
#37644=CARTESIAN_POINT('Ctrl Pts',(-11.575,-6.47446988673342,-5.01832339745483));
#37645=CARTESIAN_POINT('Ctrl Pts',(-11.575,-6.61135281749366,-4.8545366534807));
#37646=CARTESIAN_POINT('Ctrl Pts',(-11.575,-6.74167674422667,-4.68579125880677));
#37647=CARTESIAN_POINT('Ctrl Pts',(-11.575,-6.87318603173055,-4.51551104104913));
#37648=CARTESIAN_POINT('Ctrl Pts',(-11.575,-6.99801695057332,-4.34018108981283));
#37649=CARTESIAN_POINT('Ctrl Pts',(-11.575,-7.1158880737777,-4.16021989088624));
#37650=CARTESIAN_POINT('Ctrl Pts',(-11.575,-7.23343608965254,-3.98075200008146));
#37651=CARTESIAN_POINT('Ctrl Pts',(-11.575,-7.34406285148296,-3.79667767214885));
#37652=CARTESIAN_POINT('Ctrl Pts',(-11.575,-7.4474489767129,-3.60837960174284));
#37653=CARTESIAN_POINT('Ctrl Pts',(-11.575,-7.46439358665609,-3.57751823278265));
#37654=CARTESIAN_POINT('Ctrl Pts',(-11.575,-7.48114360211281,-3.54654334532797));
#37655=CARTESIAN_POINT('Ctrl Pts',(-11.575,-7.49769750071975,-3.51545655665897));
#37656=CARTESIAN_POINT('Ctrl Pts',(-11.575,-7.51133337928352,-3.48984955704557));
#37657=CARTESIAN_POINT('Ctrl Pts',(-11.575,-7.52483667088816,-3.46416559037544));
#37658=CARTESIAN_POINT('Ctrl Pts',(-11.575,-7.53819861875656,-3.43842107092718));
#37659=CARTESIAN_POINT('Ctrl Pts',(-11.575,-7.63007712735776,-3.2613983737235));
#37660=CARTESIAN_POINT('Ctrl Pts',(-11.575,-7.71536415801572,-3.08134893512341));
#37661=CARTESIAN_POINT('Ctrl Pts',(-11.575,-7.79386964549134,-2.89861723826906));
#37662=CARTESIAN_POINT('Ctrl Pts',(-11.575,-7.87843204090357,-2.70178730318278));
#37663=CARTESIAN_POINT('Ctrl Pts',(-11.575,-7.95512725273153,-2.50184530429948));
#37664=CARTESIAN_POINT('Ctrl Pts',(-11.575,-8.0239739331707,-2.29929720097265));
#37665=CARTESIAN_POINT('Ctrl Pts',(-11.575,-8.09357879607823,-2.09451851194492));
#37666=CARTESIAN_POINT('Ctrl Pts',(-11.575,-8.15516152825037,-1.88707540743478));
#37667=CARTESIAN_POINT('Ctrl Pts',(-11.575,-8.20869509004543,-1.67746392365319));
#37668=CARTESIAN_POINT('Ctrl Pts',(-11.575,-8.26244307268294,-1.46701287176828));
#37669=CARTESIAN_POINT('Ctrl Pts',(-11.575,-8.30807745914933,-1.25437538191467));
#37670=CARTESIAN_POINT('Ctrl Pts',(-11.575,-8.34552150176977,-1.04003606206454));
#37671=CARTESIAN_POINT('Ctrl Pts',(-11.575,-8.37708641586168,-0.859350384340888));
#37672=CARTESIAN_POINT('Ctrl Pts',(-11.575,-8.4028302276656,-0.677454823552394));
#37673=CARTESIAN_POINT('Ctrl Pts',(-11.575,-8.42267840796603,-0.494635356145958));
#37674=CARTESIAN_POINT('Ctrl Pts',(-11.575,-8.42653209511864,-0.459139455659049));
#37675=CARTESIAN_POINT('Ctrl Pts',(-11.575,-8.43016345121736,-0.423608722670985));
#37676=CARTESIAN_POINT('Ctrl Pts',(-11.575,-8.43357181278832,-0.388045248484162));
#37677=CARTESIAN_POINT('Ctrl Pts',(-11.575,-8.43585847597265,-0.364185782451275));
#37678=CARTESIAN_POINT('Ctrl Pts',(-11.575,-8.43804383220084,-0.340321329573578));
#37679=CARTESIAN_POINT('Ctrl Pts',(-11.575,-8.44012789284541,-0.316452872921024));
#37680=CARTESIAN_POINT('Ctrl Pts',(-11.575,-8.45926190081346,-0.0973137413588374));
#37681=CARTESIAN_POINT('Ctrl Pts',(-11.575,-8.46986214320017,0.122169579051059));
#37682=CARTESIAN_POINT('Ctrl Pts',(-11.575,-8.47193372765905,0.341484729619172));
#37683=CARTESIAN_POINT('Ctrl Pts',(-11.575,-8.47401803786911,0.562147133988573));
#37684=CARTESIAN_POINT('Ctrl Pts',(-11.575,-8.46746876336898,0.782639963557231));
#37685=CARTESIAN_POINT('Ctrl Pts',(-11.575,-8.45224135060004,1.00245787088801));
#37686=CARTESIAN_POINT('Ctrl Pts',(-11.575,-8.44874400586925,1.0529443856755));
#37687=CARTESIAN_POINT('Ctrl Pts',(-11.575,-8.44478867456793,1.10339534249771));
#37688=CARTESIAN_POINT('Ctrl Pts',(-11.575,-8.44037443380762,1.15380468310782));
#37689=CARTESIAN_POINT('Ctrl Pts',(-11.575,-8.42125072475744,1.37219185670902));
#37690=CARTESIAN_POINT('Ctrl Pts',(-11.575,-8.3935181125802,1.58979800449828));
#37691=CARTESIAN_POINT('Ctrl Pts',(-11.575,-8.35738688926969,1.80617129702421));
#37692=CARTESIAN_POINT('Ctrl Pts',(-11.575,-8.32111012297363,2.02341617960729));
#37693=CARTESIAN_POINT('Ctrl Pts',(-11.575,-8.27636680539497,2.23941890987782));
#37694=CARTESIAN_POINT('Ctrl Pts',(-11.575,-8.22331761125557,2.45371593671805));
#37695=CARTESIAN_POINT('Ctrl Pts',(-11.575,-8.19399604633327,2.57216305522919));
#37696=CARTESIAN_POINT('Ctrl Pts',(-11.575,-8.1621360953243,2.69008890813614));
#37697=CARTESIAN_POINT('Ctrl Pts',(-11.575,-8.12775833324252,2.80741327792066));
#37698=CARTESIAN_POINT('Ctrl Pts',(-11.575,-8.12030518034422,2.83284938585058));
#37699=CARTESIAN_POINT('Ctrl Pts',(-11.575,-8.11273366594586,2.85825721556884));
#37700=CARTESIAN_POINT('Ctrl Pts',(-11.575,-8.10504397159236,2.883635937813));
#37701=CARTESIAN_POINT('Ctrl Pts',(-11.575,-8.09731580645729,2.90914162729865));
#37702=CARTESIAN_POINT('Ctrl Pts',(-11.575,-8.08947069835413,2.93460986454247));
#37703=CARTESIAN_POINT('Ctrl Pts',(-11.575,-8.08151073061126,2.96003465144566));
#37704=CARTESIAN_POINT('Ctrl Pts',(-11.575,-8.01493466922925,3.17268402744423));
#37705=CARTESIAN_POINT('Ctrl Pts',(-11.575,-7.94029291252216,3.3824100176502));
#37706=CARTESIAN_POINT('Ctrl Pts',(-11.575,-7.857850150231,3.58875907821951));
#37707=CARTESIAN_POINT('Ctrl Pts',(-11.575,-7.77486600628914,3.79646318308773));
#37708=CARTESIAN_POINT('Ctrl Pts',(-11.575,-7.68397791485773,4.00074652093104));
#37709=CARTESIAN_POINT('Ctrl Pts',(-11.575,-7.58540287440055,4.20114269911254));
#37710=CARTESIAN_POINT('Ctrl Pts',(-11.575,-7.48696568741831,4.40125863079959));
#37711=CARTESIAN_POINT('Ctrl Pts',(-11.575,-7.38086282505991,4.59749892632283));
#37712=CARTESIAN_POINT('Ctrl Pts',(-11.575,-7.26726058144177,4.78938542489065));
#37713=CARTESIAN_POINT('Ctrl Pts',(-11.575,-7.20047785200925,4.90218869098355));
#37714=CARTESIAN_POINT('Ctrl Pts',(-11.575,-7.13110252862135,5.01348704406469));
#37715=CARTESIAN_POINT('Ctrl Pts',(-11.575,-7.05916078381547,5.12317972076934));
#37716=CARTESIAN_POINT('Ctrl Pts',(-11.575,-6.9600109611486,5.27435772559069));
#37717=CARTESIAN_POINT('Ctrl Pts',(-11.575,-6.85598705692301,5.42248647666084));
#37718=CARTESIAN_POINT('Ctrl Pts',(-11.575,-6.74727922420573,5.56739584840828));
#37719=CARTESIAN_POINT('Ctrl Pts',(-11.575,-6.69971954739192,5.63079369854779));
#37720=CARTESIAN_POINT('Ctrl Pts',(-11.575,-6.65126310601232,5.69357516367086));
#37721=CARTESIAN_POINT('Ctrl Pts',(-11.575,-6.6019247960547,5.7557251207176));
#37722=CARTESIAN_POINT('Ctrl Pts',(-11.575,-6.57724666313507,5.78681140847788));
#37723=CARTESIAN_POINT('Ctrl Pts',(-11.575,-6.55234789325936,5.81773969543591));
#37724=CARTESIAN_POINT('Ctrl Pts',(-11.575,-6.52723029615612,5.84850803424312));
#37725=CARTESIAN_POINT('Ctrl Pts',(-11.575,-6.51103678232919,5.86834462601018));
#37726=CARTESIAN_POINT('Ctrl Pts',(-11.575,-6.49475776389756,5.88810804101853));
#37727=CARTESIAN_POINT('Ctrl Pts',(-11.575,-6.4783961647675,5.90779520883462));
#37728=CARTESIAN_POINT('Ctrl Pts',(-11.575,-6.33570433488108,6.07948979556954));
#37729=CARTESIAN_POINT('Ctrl Pts',(-11.575,-6.18668135530418,6.24545323529948));
#37730=CARTESIAN_POINT('Ctrl Pts',(-11.575,-6.03177556639099,6.40543183256308));
#37731=CARTESIAN_POINT('Ctrl Pts',(-11.575,-5.87420677232162,6.56816064227763));
#37732=CARTESIAN_POINT('Ctrl Pts',(-11.575,-5.71055082677163,6.72469759373828));
#37733=CARTESIAN_POINT('Ctrl Pts',(-11.575,-5.54123147438693,6.87475116768693));
#37734=CARTESIAN_POINT('Ctrl Pts',(-11.575,-5.37155477858848,7.02512142520189));
#37735=CARTESIAN_POINT('Ctrl Pts',(-11.575,-5.1961902775766,7.16898140035727));
#37736=CARTESIAN_POINT('Ctrl Pts',(-11.575,-5.01552278229665,7.30600572795209));
#37737=CARTESIAN_POINT('Ctrl Pts',(-11.575,-4.83654524178164,7.44174833680182));
#37738=CARTESIAN_POINT('Ctrl Pts',(-11.575,-4.65236293303975,7.57078299743134));
#37739=CARTESIAN_POINT('Ctrl Pts',(-11.575,-4.46331662825554,7.69275536467407));
#37740=CARTESIAN_POINT('Ctrl Pts',(-11.575,-4.2770736438512,7.81291903418392));
#37741=CARTESIAN_POINT('Ctrl Pts',(-11.575,-4.08610934855102,7.92622866201986));
#37742=CARTESIAN_POINT('Ctrl Pts',(-11.575,-3.8907246099259,8.03230272149382));
#37743=CARTESIAN_POINT('Ctrl Pts',(-11.575,-4.68274545894493,-6.57070370794209));
#37744=CARTESIAN_POINT('Ctrl Pts',(-11.5441020110099,-3.83176777330803,
-7.17587091553372));
#37745=CARTESIAN_POINT('Ctrl Pts',(-11.4740577238511,-1.63517269058169,
-8.17393084810367));
#37746=CARTESIAN_POINT('Ctrl Pts',(-11.3648671385235,2.16827971646752,-8.11660023363346));
#37747=CARTESIAN_POINT('Ctrl Pts',(-11.2474282440173,5.74484511045451,-6.13001490910025));
#37748=CARTESIAN_POINT('Ctrl Pts',(-11.129989349511,7.95900894851219,-2.68972043029039));
#37749=CARTESIAN_POINT('Ctrl Pts',(-11.0125504550048,8.28568610932253,1.38846061981056));
#37750=CARTESIAN_POINT('Ctrl Pts',(-10.8951115604986,6.64740134656684,5.1373583652959));
#37751=CARTESIAN_POINT('Ctrl Pts',(-10.7776726659924,3.43267763704583,7.66792930081125));
#37752=CARTESIAN_POINT('Ctrl Pts',(-10.6602337714861,-0.596110146715297,
8.38003913890674));
#37753=CARTESIAN_POINT('Ctrl Pts',(-10.5427948769799,-4.48352951771318,
7.10481331033355));
#37754=CARTESIAN_POINT('Ctrl Pts',(-10.4253559824737,-7.3076743467974,4.14467160188776));
#37755=CARTESIAN_POINT('Ctrl Pts',(-10.3451534671224,-8.05283314175606,
1.45184169729701));
#37756=CARTESIAN_POINT('Ctrl Pts',(-10.3040972499399,-8.0691381443012,0.0645981073621665));
#37757=CARTESIAN_POINT('Ctrl Pts',(-10.3021873309261,-8.06911057618467,
6.34335902037139E-5));
#37758=CARTESIAN_POINT('Origin',(-11.575,-1.70819782223992E-15,-3.76953747432359E-16));
#37759=CARTESIAN_POINT('',(-11.575,-8.925,-1.09299726823901E-15));
#37760=CARTESIAN_POINT('Origin',(-11.575,0.,0.));
#37761=CARTESIAN_POINT('Origin',(-11.575,0.,0.));
#37762=CARTESIAN_POINT('',(-11.575,4.68253987355596,-6.5707315104605));
#37763=CARTESIAN_POINT('Ctrl Pts',(-11.575,3.8909540196873,8.03231038431327));
#37764=CARTESIAN_POINT('Ctrl Pts',(-11.575,4.09069035070338,7.92412861156293));
#37765=CARTESIAN_POINT('Ctrl Pts',(-11.575,4.28601542965074,7.80846352349093));
#37766=CARTESIAN_POINT('Ctrl Pts',(-11.575,4.4764610866747,7.6854730443605));
#37767=CARTESIAN_POINT('Ctrl Pts',(-11.575,4.54451021229802,7.64152667826528));
#37768=CARTESIAN_POINT('Ctrl Pts',(-11.575,4.61193611344074,7.59664463631333));
#37769=CARTESIAN_POINT('Ctrl Pts',(-11.575,4.67871652334774,7.55083278178531));
#37770=CARTESIAN_POINT('Ctrl Pts',(-11.575,4.86632148184985,7.42213439434502));
#37771=CARTESIAN_POINT('Ctrl Pts',(-11.575,5.0488348944294,7.28610053435785));
#37772=CARTESIAN_POINT('Ctrl Pts',(-11.575,5.22591257106765,7.14311556596555));
#37773=CARTESIAN_POINT('Ctrl Pts',(-11.575,5.34391771080921,7.04782991790192));
#37774=CARTESIAN_POINT('Ctrl Pts',(-11.575,5.45950816552951,6.94945650584669));
#37775=CARTESIAN_POINT('Ctrl Pts',(-11.575,5.57257219074754,6.84810087071603));
#37776=CARTESIAN_POINT('Ctrl Pts',(-11.575,5.61416040373507,6.81081934166051));
#37777=CARTESIAN_POINT('Ctrl Pts',(-11.575,5.65540671294731,6.77313426639739));
#37778=CARTESIAN_POINT('Ctrl Pts',(-11.575,5.69630525962318,6.73505070840406));
#37779=CARTESIAN_POINT('Ctrl Pts',(-11.575,5.72899935727988,6.70460689889619));
#37780=CARTESIAN_POINT('Ctrl Pts',(-11.575,5.76147534498076,6.67390437527803));
#37781=CARTESIAN_POINT('Ctrl Pts',(-11.575,5.79370643387823,6.64296877678564));
#37782=CARTESIAN_POINT('Ctrl Pts',(-11.575,5.95657310025678,6.48664834296758));
#37783=CARTESIAN_POINT('Ctrl Pts',(-11.575,6.11328907427985,6.32428998283107));
#37784=CARTESIAN_POINT('Ctrl Pts',(-11.575,6.2635341324018,6.15628508681688));
#37785=CARTESIAN_POINT('Ctrl Pts',(-11.575,6.41336099455174,5.98874781996579));
#37786=CARTESIAN_POINT('Ctrl Pts',(-11.575,6.55675331297687,5.81559485699136));
#37787=CARTESIAN_POINT('Ctrl Pts',(-11.575,6.69335279993625,5.63718293709442));
#37788=CARTESIAN_POINT('Ctrl Pts',(-11.575,6.82873374273438,5.46036255174955));
#37789=CARTESIAN_POINT('Ctrl Pts',(-11.575,6.95744284599461,5.27837607658992));
#37790=CARTESIAN_POINT('Ctrl Pts',(-11.575,7.07908582397012,5.09154805860869));
#37791=CARTESIAN_POINT('Ctrl Pts',(-11.575,7.10207551861353,5.05623883520997));
#37792=CARTESIAN_POINT('Ctrl Pts',(-11.575,7.12481268216614,5.02075662710973));
#37793=CARTESIAN_POINT('Ctrl Pts',(-11.575,7.14729445264254,4.9851035570856));
#37794=CARTESIAN_POINT('Ctrl Pts',(-11.575,7.1681591197164,4.95201499597806));
#37795=CARTESIAN_POINT('Ctrl Pts',(-11.575,7.18880670503735,4.91877440480665));
#37796=CARTESIAN_POINT('Ctrl Pts',(-11.575,7.20921801861532,4.88541141690287));
#37797=CARTESIAN_POINT('Ctrl Pts',(-11.575,7.31755469203634,4.70833143079254));
#37798=CARTESIAN_POINT('Ctrl Pts',(-11.575,7.41931816251136,4.52768181901124));
#37799=CARTESIAN_POINT('Ctrl Pts',(-11.575,7.51425932679982,4.3437592816672));
#37800=CARTESIAN_POINT('Ctrl Pts',(-11.575,7.61605469031111,4.14655860810088));
#37801=CARTESIAN_POINT('Ctrl Pts',(-11.575,7.71000799576338,3.94559518439185));
#37802=CARTESIAN_POINT('Ctrl Pts',(-11.575,7.79604523983125,3.74136883761279));
#37803=CARTESIAN_POINT('Ctrl Pts',(-11.575,7.88244746162894,3.53627614429712));
#37804=CARTESIAN_POINT('Ctrl Pts',(-11.575,7.96086647438103,3.3278921106263));
#37805=CARTESIAN_POINT('Ctrl Pts',(-11.575,8.03117746555899,3.11670639005853));
#37806=CARTESIAN_POINT('Ctrl Pts',(-11.575,8.10121298627027,2.90634807112496));
#37807=CARTESIAN_POINT('Ctrl Pts',(-11.575,8.1632039896943,2.69320929856103));
#37808=CARTESIAN_POINT('Ctrl Pts',(-11.575,8.21697596967883,2.4777677535818));
#37809=CARTESIAN_POINT('Ctrl Pts',(-11.575,8.26188761707955,2.29782580786291));
#37810=CARTESIAN_POINT('Ctrl Pts',(-11.575,8.30106482476432,2.11627714880915));
#37811=CARTESIAN_POINT('Ctrl Pts',(-11.575,8.33437760016051,1.93340186433423));
#37812=CARTESIAN_POINT('Ctrl Pts',(-11.575,8.3410674207946,1.89667712924399));
#37813=CARTESIAN_POINT('Ctrl Pts',(-11.575,8.34752065536839,1.85989890749364));
#37814=CARTESIAN_POINT('Ctrl Pts',(-11.575,8.35373612235081,1.82306949144067));
#37815=CARTESIAN_POINT('Ctrl Pts',(-11.575,8.35791106064617,1.79833111861849));
#37816=CARTESIAN_POINT('Ctrl Pts',(-11.575,8.36197777909343,1.7735750980682));
#37817=CARTESIAN_POINT('Ctrl Pts',(-11.575,8.3659349176602,1.74880967041789));
#37818=CARTESIAN_POINT('Ctrl Pts',(-11.575,8.40065470151849,1.53151874651718));
#37819=CARTESIAN_POINT('Ctrl Pts',(-11.575,8.42697311679527,1.31332666260153));
#37820=CARTESIAN_POINT('Ctrl Pts',(-11.575,8.44480476752567,1.09470887941076));
#37821=CARTESIAN_POINT('Ctrl Pts',(-11.575,8.46257370213098,0.876860002051726));
#37822=CARTESIAN_POINT('Ctrl Pts',(-11.575,8.47191553606587,0.65858774848646));
#37823=CARTESIAN_POINT('Ctrl Pts',(-11.575,8.47269453239138,0.440357329235993));
#37824=CARTESIAN_POINT('Ctrl Pts',(-11.575,8.47289362379682,0.384583252443501));
#37825=CARTESIAN_POINT('Ctrl Pts',(-11.575,8.47253314142673,0.328811909903161));
#37826=CARTESIAN_POINT('Ctrl Pts',(-11.575,8.47161027062858,0.273051092863091));
#37827=CARTESIAN_POINT('Ctrl Pts',(-11.575,8.46798133197079,0.0537868307881026));
#37828=CARTESIAN_POINT('Ctrl Pts',(-11.575,8.4556604711072,-0.165315593783987));
#37829=CARTESIAN_POINT('Ctrl Pts',(-11.575,8.43476764154084,-0.383762556599518));
#37830=CARTESIAN_POINT('Ctrl Pts',(-11.575,8.41395932183961,-0.601325918497957));
#37831=CARTESIAN_POINT('Ctrl Pts',(-11.575,8.3846480034043,-0.818239764904438));
#37832=CARTESIAN_POINT('Ctrl Pts',(-11.575,8.34690369724573,-1.03399926810862));
#37833=CARTESIAN_POINT('Ctrl Pts',(-11.575,8.32669936168747,-1.14949423533114));
#37834=CARTESIAN_POINT('Ctrl Pts',(-11.575,8.30407782627792,-1.26465808454184));
#37835=CARTESIAN_POINT('Ctrl Pts',(-11.575,8.27904443208135,-1.37941035657947));
#37836=CARTESIAN_POINT('Ctrl Pts',(-11.575,8.27346937299148,-1.40496624773363));
#37837=CARTESIAN_POINT('Ctrl Pts',(-11.575,8.26777467745199,-1.4305017159728));
#37838=CARTESIAN_POINT('Ctrl Pts',(-11.575,8.26196037991734,-1.45601585527642));
#37839=CARTESIAN_POINT('Ctrl Pts',(-11.575,8.25632839154964,-1.48072999054615));
#37840=CARTESIAN_POINT('Ctrl Pts',(-11.575,8.25058629462981,-1.50541481702675));
#37841=CARTESIAN_POINT('Ctrl Pts',(-11.575,8.24473496759404,-1.53006711391079));
#37842=CARTESIAN_POINT('Ctrl Pts',(-11.575,8.19462468872943,-1.74118733740221));
#37843=CARTESIAN_POINT('Ctrl Pts',(-11.575,8.13649408842284,-1.94998221456258));
#37844=CARTESIAN_POINT('Ctrl Pts',(-11.575,8.07050941331969,-2.15598886710096));
#37845=CARTESIAN_POINT('Ctrl Pts',(-11.575,8.00454781312325,-2.36192347890745));
#37846=CARTESIAN_POINT('Ctrl Pts',(-11.575,7.93073739624093,-2.56507246994707));
#37847=CARTESIAN_POINT('Ctrl Pts',(-11.575,7.8491944550522,-2.76495843616166));
#37848=CARTESIAN_POINT('Ctrl Pts',(-11.575,7.7685709179915,-2.96259066980547));
#37849=CARTESIAN_POINT('Ctrl Pts',(-11.575,7.68038795006705,-3.15703362359616));
#37850=CARTESIAN_POINT('Ctrl Pts',(-11.575,7.58471333576317,-3.34780208001595));
#37851=CARTESIAN_POINT('Ctrl Pts',(-11.575,7.53014632821733,-3.45660485781346));
#37852=CARTESIAN_POINT('Ctrl Pts',(-11.575,7.47314159064295,-3.56421188609963));
#37853=CARTESIAN_POINT('Ctrl Pts',(-11.575,7.41370561910289,-3.67052853101672));
#37854=CARTESIAN_POINT('Ctrl Pts',(-11.575,7.33195298620427,-3.81676431075931));
#37855=CARTESIAN_POINT('Ctrl Pts',(-11.575,7.24560098255595,-3.96055936581355));
#37856=CARTESIAN_POINT('Ctrl Pts',(-11.575,7.1547904636629,-4.10172616067142));
#37857=CARTESIAN_POINT('Ctrl Pts',(-11.575,7.11506086164719,-4.16348663342174));
#37858=CARTESIAN_POINT('Ctrl Pts',(-11.575,7.07447771520422,-4.22474385495871));
#37859=CARTESIAN_POINT('Ctrl Pts',(-11.575,7.03305213420888,-4.28548120740034));
#37860=CARTESIAN_POINT('Ctrl Pts',(-11.575,7.00995571903755,-4.31934470610558));
#37861=CARTESIAN_POINT('Ctrl Pts',(-11.575,6.98659742541435,-4.35304659275271));
#37862=CARTESIAN_POINT('Ctrl Pts',(-11.575,6.96297912814017,-4.38658390647314));
#37863=CARTESIAN_POINT('Ctrl Pts',(-11.575,6.94725346269133,-4.40891390636678));
#37864=CARTESIAN_POINT('Ctrl Pts',(-11.575,6.93141725469661,-4.43116419555797));
#37865=CARTESIAN_POINT('Ctrl Pts',(-11.575,6.91547562163386,-4.45332807617772));
#37866=CARTESIAN_POINT('Ctrl Pts',(-11.575,6.79134840278254,-4.62590392517971));
#37867=CARTESIAN_POINT('Ctrl Pts',(-11.575,6.66075184134787,-4.79335902618009));
#37868=CARTESIAN_POINT('Ctrl Pts',(-11.575,6.52405945291491,-4.95538312636472));
#37869=CARTESIAN_POINT('Ctrl Pts',(-11.575,6.38652067756353,-5.11841046513812));
#37870=CARTESIAN_POINT('Ctrl Pts',(-11.575,6.2428098747442,-5.27593983973574));
#37871=CARTESIAN_POINT('Ctrl Pts',(-11.575,6.09326686075735,-5.42762206125614));
#37872=CARTESIAN_POINT('Ctrl Pts',(-11.575,5.94445087436889,-5.57856685507403));
#37873=CARTESIAN_POINT('Ctrl Pts',(-11.575,5.78985872238046,-5.72372164315627));
#37874=CARTESIAN_POINT('Ctrl Pts',(-11.575,5.62979274260417,-5.86270269648403));
#37875=CARTESIAN_POINT('Ctrl Pts',(-11.575,5.47264807795008,-5.99914724921779));
#37876=CARTESIAN_POINT('Ctrl Pts',(-11.575,5.31022703737972,-6.12964166221526));
#37877=CARTESIAN_POINT('Ctrl Pts',(-11.575,5.14279211761008,-6.25377930689961));
#37878=CARTESIAN_POINT('Ctrl Pts',(-11.575,4.99331293730095,-6.36460441673007));
#37879=CARTESIAN_POINT('Ctrl Pts',(-11.575,4.83983707019304,-6.47036267996695));
#37880=CARTESIAN_POINT('Ctrl Pts',(-11.575,4.68253987355598,-6.57073151046049));
#37881=CARTESIAN_POINT('Origin',(-11.575,0.,0.));
#37882=CARTESIAN_POINT('Origin',(-14.3478126690739,0.,0.));
#37883=CARTESIAN_POINT('Ctrl Pts',(-11.575,4.68253987355595,-6.57073151046051));
#37884=CARTESIAN_POINT('Ctrl Pts',(-11.5358537018313,5.75997971466614,-5.80290908318214));
#37885=CARTESIAN_POINT('Ctrl Pts',(-11.4575611054938,7.52902184303394,-3.72801696096832));
#37886=CARTESIAN_POINT('Ctrl Pts',(-11.3401222109875,8.39684879745447,0.270811863526706));
#37887=CARTESIAN_POINT('Ctrl Pts',(-11.2226833164813,7.27339149706363,4.20443640376082));
#37888=CARTESIAN_POINT('Ctrl Pts',(-11.1052444219751,4.42502579862193,7.14145324703773));
#37889=CARTESIAN_POINT('Ctrl Pts',(-10.9878055274688,0.527266627263149,
8.38462365194841));
#37890=CARTESIAN_POINT('Ctrl Pts',(-10.8703666329626,-3.49553795222623,
7.63949276732611));
#37891=CARTESIAN_POINT('Ctrl Pts',(-10.7529277384564,-6.68936958853091,
5.08258437974203));
#37892=CARTESIAN_POINT('Ctrl Pts',(-10.6620764171601,-7.93289342748698,
2.17211355225587));
#37893=CARTESIAN_POINT('Ctrl Pts',(-10.6103713940326,-8.0685071350501,0.424666440026747));
#37894=CARTESIAN_POINT('Ctrl Pts',(-10.5978126690739,-8.06816497465237,
0.000173167597293036));
#37895=CARTESIAN_POINT('Ctrl Pts',(-12.0695005055609,5.17960815163744,-7.26823805302846));
#37896=CARTESIAN_POINT('Ctrl Pts',(-12.0303542073922,6.37142206771955,-6.41890854153817));
#37897=CARTESIAN_POINT('Ctrl Pts',(-11.9520616110547,8.32825431605352,-4.12375923364224));
#37898=CARTESIAN_POINT('Ctrl Pts',(-11.8346227165484,9.28820419127237,0.299559506968546));
#37899=CARTESIAN_POINT('Ctrl Pts',(-11.7171838220422,8.04548789877833,4.65075229640766));
#37900=CARTESIAN_POINT('Ctrl Pts',(-11.599744927536,4.89475804086272,7.89954393379335));
#37901=CARTESIAN_POINT('Ctrl Pts',(-11.4823060330297,0.583237856890839,
9.2746813030476));
#37902=CARTESIAN_POINT('Ctrl Pts',(-11.3648671385235,-3.86660175046402,
8.45045212225142));
#37903=CARTESIAN_POINT('Ctrl Pts',(-11.2474282440173,-7.39946998545434,
5.62211880637018));
#37904=CARTESIAN_POINT('Ctrl Pts',(-11.1299893495111,-9.17754567157279,
1.4605279695957));
#37905=CARTESIAN_POINT('Ctrl Pts',(-11.0125504550048,-8.77915445415917,
-3.04744664874868));
#37906=CARTESIAN_POINT('Ctrl Pts',(-10.8951115604986,-6.29877606274185,
-6.83270648092648));
#37907=CARTESIAN_POINT('Ctrl Pts',(-10.7776726659923,-2.32463494290788,
-8.99758602485665));
#37908=CARTESIAN_POINT('Ctrl Pts',(-10.6602337714861,2.20079618741207,-9.0286744979603));
#37909=CARTESIAN_POINT('Ctrl Pts',(-10.5427948769799,6.20430579028754,-6.91860273246797));
#37910=CARTESIAN_POINT('Ctrl Pts',(-10.4253559824737,8.7364565199315,-3.16777510115142));
#37911=CARTESIAN_POINT('Ctrl Pts',(-10.3079170879674,9.1967456981277,1.33429404234123));
#37912=CARTESIAN_POINT('Ctrl Pts',(-10.1904781934612,7.47601515924667,5.5199338438618));
#37913=CARTESIAN_POINT('Ctrl Pts',(-10.073039298955,3.98233830328959,8.39651437135721));
#37914=CARTESIAN_POINT('Ctrl Pts',(-9.95560040444873,-0.455755049286878,
9.28185108312358));
#37915=CARTESIAN_POINT('Ctrl Pts',(-9.83816150994249,-4.78576552292591,
7.96598521377529));
#37916=CARTESIAN_POINT('Ctrl Pts',(-9.72072261543627,-7.98082573416653,
4.76097602585856));
#37917=CARTESIAN_POINT('Ctrl Pts',(-9.60328372093003,-9.28322316851808,
0.426895430196007));
#37918=CARTESIAN_POINT('Ctrl Pts',(-9.4858448264238,-8.38409265026308,-4.00842394652925));
#37919=CARTESIAN_POINT('Ctrl Pts',(-9.36840593191757,-5.49666410311126,
-7.49314058627073));
#37920=CARTESIAN_POINT('Ctrl Pts',(-9.25096703741133,-1.30569480834948,
-9.2008495896654));
#37921=CARTESIAN_POINT('Ctrl Pts',(-9.13352814290511,3.19492163871721,-8.72656563768809));
#37922=CARTESIAN_POINT('Ctrl Pts',(-9.01608924839887,6.93785843437135,-6.18276576056752));
#37923=CARTESIAN_POINT('Ctrl Pts',(-8.89865035389264,9.03547344924704,-2.17271527211811));
#37924=CARTESIAN_POINT('Ctrl Pts',(-8.78121145938641,8.9903146663651,2.35259735302393));
#37925=CARTESIAN_POINT('Ctrl Pts',(-8.66377256488017,6.81309154741103,6.31998858165539));
#37926=CARTESIAN_POINT('Ctrl Pts',(-8.54633367037394,3.0201352705307,8.78858663571183));
#37927=CARTESIAN_POINT('Ctrl Pts',(-8.42889477586771,-1.48904985254373,
9.17296040775923));
#37928=CARTESIAN_POINT('Ctrl Pts',(-8.31145588136147,-5.64510494590745,
7.38195517836491));
#37929=CARTESIAN_POINT('Ctrl Pts',(-8.19401698685524,-8.46241636063372,
3.84031007146154));
#37930=CARTESIAN_POINT('Ctrl Pts',(-8.07657809234901,-9.27285518089936,
-0.612069358618491));
#37931=CARTESIAN_POINT('Ctrl Pts',(-7.95913919784278,-7.88422482967884,
-4.9192957769144));
#37932=CARTESIAN_POINT('Ctrl Pts',(-7.84170030333655,-4.6258407266985,-8.05990506624669));
#37933=CARTESIAN_POINT('Ctrl Pts',(-7.72426140883031,-0.270432725917864,
-9.28909781660439));
#37934=CARTESIAN_POINT('Ctrl Pts',(-7.60682251432408,4.14910873310461,-8.31536943416027));
#37935=CARTESIAN_POINT('Ctrl Pts',(-7.48938361981784,7.58468388119963,-5.36964081926924));
#37936=CARTESIAN_POINT('Ctrl Pts',(-7.37194472531162,9.22154178706155,-1.1504951869388));
#37937=CARTESIAN_POINT('Ctrl Pts',(-7.25450583080538,8.67149955678534,3.34149181390041));
#37938=CARTESIAN_POINT('Ctrl Pts',(-7.13706693629915,6.06500039130734,7.04103986348135));
#37939=CARTESIAN_POINT('Ctrl Pts',(-7.01962804179292,2.02017881861132,9.0707965276775));
#37940=CARTESIAN_POINT('Ctrl Pts',(-6.90218914728668,-2.50373068053572,
8.94940248201162));
#37941=CARTESIAN_POINT('Ctrl Pts',(-6.78475025278046,-6.43387732607846,
6.70564647581913));
#37942=CARTESIAN_POINT('Ctrl Pts',(-6.66731135827422,-8.83822193924971,
2.87163804443684));
#37943=CARTESIAN_POINT('Ctrl Pts',(-6.54987246376798,-9.14657119627741,
-1.64338293076208));
#37944=CARTESIAN_POINT('Ctrl Pts',(-6.43243356926176,-7.28579968627662,
-5.76867359426266));
#37945=CARTESIAN_POINT('Ctrl Pts',(-6.31499467475552,-3.69719169364456,
-8.52591612005052));
#37946=CARTESIAN_POINT('Ctrl Pts',(-6.1975557802493,0.768209920364817,-9.26122700423357));
#37947=CARTESIAN_POINT('Ctrl Pts',(-6.08011688574306,5.05142959362918,-7.8002263535297));
#37948=CARTESIAN_POINT('Ctrl Pts',(-5.96267799123683,8.1366964384956,-4.48939229444975));
#37949=CARTESIAN_POINT('Ctrl Pts',(-5.8452390967306,9.29233557468242,-0.113893253459215));
#37950=CARTESIAN_POINT('Ctrl Pts',(-5.72780020222436,8.24428573970098,4.28861571463967));
#37951=CARTESIAN_POINT('Ctrl Pts',(-5.61036130771813,5.24109325907115,7.67407411714348));
#37952=CARTESIAN_POINT('Ctrl Pts',(-5.4929224132119,0.994968975230345,9.23961627147041));
#37953=CARTESIAN_POINT('Ctrl Pts',(-5.37548351870567,-3.487113442036,8.61397190313867));
#37954=CARTESIAN_POINT('Ctrl Pts',(-5.25804462419943,-7.14222255730959,
5.94551335441738));
#37955=CARTESIAN_POINT('Ctrl Pts',(-5.14060572969321,-9.10354468515787,
1.86706889830364));
#37956=CARTESIAN_POINT('Ctrl Pts',(-5.02316683518696,-8.90594983675637,
-2.65415327569744));
#37957=CARTESIAN_POINT('Ctrl Pts',(-4.90572794068074,-6.5962978768398,-6.5459396900412));
#37958=CARTESIAN_POINT('Ctrl Pts',(-4.7882890461745,-2.72232564837539,-8.88534834263194));
#37959=CARTESIAN_POINT('Ctrl Pts',(-4.67085015166827,1.79724950297649,-9.11758555374142));
#37960=CARTESIAN_POINT('Ctrl Pts',(-4.55341125716204,5.89060469307803,-7.18757597909831));
#37961=CARTESIAN_POINT('Ctrl Pts',(-4.43597236265581,8.58699563339623,-3.55302379649448));
#37962=CARTESIAN_POINT('Ctrl Pts',(-4.31853346814957,9.24696984916455,0.924132410879959));
#37963=CARTESIAN_POINT('Ctrl Pts',(-4.20109457364334,7.7140136324976,5.18212946438919));
#37964=CARTESIAN_POINT('Ctrl Pts',(-4.08365567913711,4.35166946109418,8.21117805218502));
#37965=CARTESIAN_POINT('Ctrl Pts',(-3.96621678463088,-0.0426785491791672,
9.29293552362616));
#37966=CARTESIAN_POINT('Ctrl Pts',(-3.84877789012465,-4.42690529092247,
8.17086174544261));
#37967=CARTESIAN_POINT('Ctrl Pts',(-3.73133899561841,-7.76128591638191,
5.11105791306308));
#37968=CARTESIAN_POINT('Ctrl Pts',(-3.61390010111218,-9.25506791693505,
0.839160322675105));
#37969=CARTESIAN_POINT('Ctrl Pts',(-3.49646120660595,-8.55399899768065,
-3.63174518626155));
#37970=CARTESIAN_POINT('Ctrl Pts',(-3.37902231209972,-5.82433858706542,
-7.24137779190658));
#37971=CARTESIAN_POINT('Ctrl Pts',(-3.26158341759348,-1.71342893807153,
-9.13370862802382));
#37972=CARTESIAN_POINT('Ctrl Pts',(-3.14414452308726,2.80382236659545,-8.85996906048253));
#37973=CARTESIAN_POINT('Ctrl Pts',(-3.02670562858102,6.65614400340243,-6.4850768010162));
#37974=CARTESIAN_POINT('Ctrl Pts',(-2.90926673407479,8.92995219053902,-2.5722404481956));
#37975=CARTESIAN_POINT('Ctrl Pts',(-2.79182783956855,9.08601225502845,1.95060585305106));
#37976=CARTESIAN_POINT('Ctrl Pts',(-2.67438894506232,7.08731086261654,6.01086370496802));
#37977=CARTESIAN_POINT('Ctrl Pts',(-2.55695005055609,3.40784942603698,8.64563741411886));
#37978=CARTESIAN_POINT('Ctrl Pts',(-2.43951115604986,-1.07979674662018,
9.23008805428009));
#37979=CARTESIAN_POINT('Ctrl Pts',(-2.32207226154363,-5.31135005799377,
7.62561056572066));
#37980=CARTESIAN_POINT('Ctrl Pts',(-2.20463336703739,-8.28334497403523,
4.21271245259873));
#37981=CARTESIAN_POINT('Ctrl Pts',(-2.08719447253116,-9.29086556292747,
-0.199240463811235));
#37982=CARTESIAN_POINT('Ctrl Pts',(-1.96975557802493,-8.09518120960245,
-4.56393381023661));
#37983=CARTESIAN_POINT('Ctrl Pts',(-1.8523166835187,-4.97944750926598,-7.84630326678714));
#37984=CARTESIAN_POINT('Ctrl Pts',(-1.73487778901247,-0.683361058726897,
-9.26787411763888));
#37985=CARTESIAN_POINT('Ctrl Pts',(-1.61743889450623,3.77586765201595,-8.49164493160031));
#37986=CARTESIAN_POINT('Ctrl Pts',(-1.53914629816874,6.14996708109111,-6.63138831099122));
#37987=CARTESIAN_POINT('Ctrl Pts',(-1.5,7.04785050324084,-5.47571258230085));
#37988=CARTESIAN_POINT('Ctrl Pts',(-11.9046670037073,5.01391872561028,-7.03573587217248));
#37989=CARTESIAN_POINT('Ctrl Pts',(-11.8655207055385,6.16760795003508,-6.21357538875283));
#37990=CARTESIAN_POINT('Ctrl Pts',(-11.787228109201,8.06184349171365,-3.99184514275093));
#37991=CARTESIAN_POINT('Ctrl Pts',(-11.6697892146948,8.99108572666641,0.289976959154598));
#37992=CARTESIAN_POINT('Ctrl Pts',(-11.5523503201886,7.7881224315401,4.50198033219205));
#37993=CARTESIAN_POINT('Ctrl Pts',(-11.4349114256823,4.73818062678245,7.64684703820814));
#37994=CARTESIAN_POINT('Ctrl Pts',(-11.3174725311761,0.564580780348278,
8.97799541934787));
#37995=CARTESIAN_POINT('Ctrl Pts',(-11.2000336366699,-3.7429138177181,8.18013233727632));
#37996=CARTESIAN_POINT('Ctrl Pts',(-11.0825947421636,-7.16276985314653,
5.44227399749412));
#37997=CARTESIAN_POINT('Ctrl Pts',(-10.9651558476574,-8.88396703972585,
1.41380743902767));
#37998=CARTESIAN_POINT('Ctrl Pts',(-10.8477169531512,-8.4983198775023,-2.94996250104922));
#37999=CARTESIAN_POINT('Ctrl Pts',(-10.730278058645,-6.09728580325582,-6.6141364304722));
#38000=CARTESIAN_POINT('Ctrl Pts',(-10.6128391641387,-2.25027267106471,
-8.70976408535003));
#38001=CARTESIAN_POINT('Ctrl Pts',(-10.4954002696325,2.1303953681957,-8.73985807564459));
#38002=CARTESIAN_POINT('Ctrl Pts',(-10.3779613751262,6.00583752102961,-6.69728496438734));
#38003=CARTESIAN_POINT('Ctrl Pts',(-10.26052248062,8.4569877987617,-3.06644179119301));
#38004=CARTESIAN_POINT('Ctrl Pts',(-10.1430835861138,8.90255288055735,1.29161158305961));
#38005=CARTESIAN_POINT('Ctrl Pts',(-10.0256446916076,7.2368664390265,5.34335780885649));
#38006=CARTESIAN_POINT('Ctrl Pts',(-9.90820579710132,3.85494809762134,8.12791999006617));
#38007=CARTESIAN_POINT('Ctrl Pts',(-9.79076690259508,-0.44117599420886,
8.9849358467951));
#38008=CARTESIAN_POINT('Ctrl Pts',(-9.67332800808886,-4.63267464821495,
7.71116294167077));
#38009=CARTESIAN_POINT('Ctrl Pts',(-9.55588911358262,-7.72552873168984,
4.60867813730028));
#38010=CARTESIAN_POINT('Ctrl Pts',(-9.43845021907639,-8.98626404083047,
0.413239559571804));
#38011=CARTESIAN_POINT('Ctrl Pts',(-9.32101132457016,-8.11589562486812,
-3.88019929255345));
#38012=CARTESIAN_POINT('Ctrl Pts',(-9.20357243006392,-5.32083243908456,
-7.25344404426735));
#38013=CARTESIAN_POINT('Ctrl Pts',(-9.0861335355577,-1.263927204116,-8.90652549354782));
#38014=CARTESIAN_POINT('Ctrl Pts',(-8.96869464105145,3.09271994371959,-8.44741331392787));
#38015=CARTESIAN_POINT('Ctrl Pts',(-8.85125574654525,6.71592469957997,-5.98498653091574));
#38016=CARTESIAN_POINT('Ctrl Pts',(-8.73381685203898,8.7464395366689,-2.10321272755903));
#38017=CARTESIAN_POINT('Ctrl Pts',(-8.61637795753279,8.7027253288584,2.27734059736138));
#38018=CARTESIAN_POINT('Ctrl Pts',(-8.49893906302652,6.59514895505407,6.11781975923941));
#38019=CARTESIAN_POINT('Ctrl Pts',(-8.38150016852031,2.92352478092436,8.507450334928));
#38020=CARTESIAN_POINT('Ctrl Pts',(-8.26406127401406,-1.4414169412943,8.8795284529788));
#38021=CARTESIAN_POINT('Ctrl Pts',(-8.14662237950784,-5.464524838114,7.14581532363963));
#38022=CARTESIAN_POINT('Ctrl Pts',(-8.0291834850016,-8.19171385408349,3.71746317785904));
#38023=CARTESIAN_POINT('Ctrl Pts',(-7.91174459049538,-8.97622771264762,
-0.592489997062687));
#38024=CARTESIAN_POINT('Ctrl Pts',(-7.79430569598914,-7.63201797378267,
-4.76193343021311));
#38025=CARTESIAN_POINT('Ctrl Pts',(-7.67686680148291,-4.47786565359234,
-7.80207841118636));
#38026=CARTESIAN_POINT('Ctrl Pts',(-7.55942790697667,-0.261781908747044,
-8.99195076600041));
#38027=CARTESIAN_POINT('Ctrl Pts',(-7.44198901247044,4.01638374225852,-8.04937078167256));
#38028=CARTESIAN_POINT('Ctrl Pts',(-7.32455011796421,7.34205897945369,-5.19787247709541));
#38029=CARTESIAN_POINT('Ctrl Pts',(-7.20711122345798,8.92655577247263,-1.11369223165913));
#38030=CARTESIAN_POINT('Ctrl Pts',(-7.08967232895174,8.39410873062712,3.2346015155398));
#38031=CARTESIAN_POINT('Ctrl Pts',(-6.97223343444552,5.87098833397195,6.81580547905291));
#38032=CARTESIAN_POINT('Ctrl Pts',(-6.85479453993928,1.95555573147255,8.78063267236637));
#38033=CARTESIAN_POINT('Ctrl Pts',(-6.73735564543305,-2.42363935176341,
8.66312187600441));
#38034=CARTESIAN_POINT('Ctrl Pts',(-6.61991675092681,-6.22806533990531,
6.49114092188676));
#38035=CARTESIAN_POINT('Ctrl Pts',(-6.50247785642058,-8.55549786489052,
2.77977780223104));
#38036=CARTESIAN_POINT('Ctrl Pts',(-6.38503896191435,-8.85398340058697,
-1.59081309023183));
#38037=CARTESIAN_POINT('Ctrl Pts',(-6.26760006740812,-7.05273572992569,
-5.58414067424452));
#38038=CARTESIAN_POINT('Ctrl Pts',(-6.15016117290189,-3.57892298456495,
-8.25318233268084));
#38039=CARTESIAN_POINT('Ctrl Pts',(-6.03272227839566,0.743635810307214,
-8.96497150734744));
#38040=CARTESIAN_POINT('Ctrl Pts',(-5.91528338388941,4.88984044528396,-7.5507065077109));
#38041=CARTESIAN_POINT('Ctrl Pts',(-5.79784448938319,7.87641331993083,-4.34578204234158));
#38042=CARTESIAN_POINT('Ctrl Pts',(-5.68040559487695,8.99508495209735,-0.110249945463397));
#38043=CARTESIAN_POINT('Ctrl Pts',(-5.56296670037073,7.98056096898001,4.1514280634879));
#38044=CARTESIAN_POINT('Ctrl Pts',(-5.44552780586449,5.07343699851486,7.42858972941861));
#38045=CARTESIAN_POINT('Ctrl Pts',(-5.32808891135826,0.963141116134738,
8.94405207589564));
#38046=CARTESIAN_POINT('Ctrl Pts',(-5.21065001685203,-3.37556488318993,
8.33842131732958));
#38047=CARTESIAN_POINT('Ctrl Pts',(-5.09321112234579,-6.91375146037828,
5.75532354347215));
#38048=CARTESIAN_POINT('Ctrl Pts',(-4.97577222783957,-8.8123332557335,1.80734361309739));
#38049=CARTESIAN_POINT('Ctrl Pts',(-4.85833333333333,-8.62105922853295,
-2.56925010928718));
#38050=CARTESIAN_POINT('Ctrl Pts',(-4.7408944388271,-6.38529025288039,-6.33654296382196));
#38051=CARTESIAN_POINT('Ctrl Pts',(-4.62345554432087,-2.63524172987553,
-8.60111675139145));
#38052=CARTESIAN_POINT('Ctrl Pts',(-4.50601664981463,1.73975765613059,-8.82592497384302));
#38053=CARTESIAN_POINT('Ctrl Pts',(-4.3885777553084,5.70217134407256,-6.95765408083135));
#38054=CARTESIAN_POINT('Ctrl Pts',(-4.27113886080217,8.31230798596378,-3.43936684479708));
#38055=CARTESIAN_POINT('Ctrl Pts',(-4.15369996629594,8.9511704214966,0.894570528156575));
#38056=CARTESIAN_POINT('Ctrl Pts',(-4.0362610717897,7.46725162778297,5.01635938460398));
#38057=CARTESIAN_POINT('Ctrl Pts',(-3.91882217728347,4.21246479654041,7.94851235651008));
#38058=CARTESIAN_POINT('Ctrl Pts',(-3.80138328277724,-0.0413133137964638,
8.99566570939701));
#38059=CARTESIAN_POINT('Ctrl Pts',(-3.68394438827101,-4.28529392279269,
7.9094857198601));
#38060=CARTESIAN_POINT('Ctrl Pts',(-3.56650549376477,-7.51301172824443,
4.94756132660039));
#38061=CARTESIAN_POINT('Ctrl Pts',(-3.44906659925855,-8.9590094418331,0.812316594706053));
#38062=CARTESIAN_POINT('Ctrl Pts',(-3.33162770475231,-8.28036687288089,
-3.515570032124));
#38063=CARTESIAN_POINT('Ctrl Pts',(-3.21418881024608,-5.63802501097498,
-7.0097348384512));
#38064=CARTESIAN_POINT('Ctrl Pts',(-3.09674991573984,-1.65861841013657,
-8.84153229039908));
#38065=CARTESIAN_POINT('Ctrl Pts',(-2.97931102123362,2.71413146624106,-8.57654932190911));
#38066=CARTESIAN_POINT('Ctrl Pts',(-2.86187212672738,6.44322197393785,-6.27762700530862));
#38067=CARTESIAN_POINT('Ctrl Pts',(-2.74443323222115,8.6442937759285,-2.4899575744746));
#38068=CARTESIAN_POINT('Ctrl Pts',(-2.62699433771492,8.79536166692642,1.8882083212812));
#38069=CARTESIAN_POINT('Ctrl Pts',(-2.50955544320868,6.86059632465833,5.81858341502198));
#38070=CARTESIAN_POINT('Ctrl Pts',(-2.39211654870245,3.29883642759064,8.36907388675404));
#38071=CARTESIAN_POINT('Ctrl Pts',(-2.27467765419622,-1.04525534929133,
8.93482865489668));
#38072=CARTESIAN_POINT('Ctrl Pts',(-2.15723875968999,-5.14144636706299,
7.38167646863233));
#38073=CARTESIAN_POINT('Ctrl Pts',(-2.03979986518375,-8.01837074545405,
4.07795285537554));
#38074=CARTESIAN_POINT('Ctrl Pts',(-1.92236097067752,-8.99366196424782,
-0.192867001355429));
#38075=CARTESIAN_POINT('Ctrl Pts',(-1.80492207617129,-7.83622611320565,
-4.41793906482233));
#38076=CARTESIAN_POINT('Ctrl Pts',(-1.68748318166506,-4.82016098109842,
-7.59530947601204));
#38077=CARTESIAN_POINT('Ctrl Pts',(-1.57004428715883,-0.661501161554172,
-8.97140598760125));
#38078=CARTESIAN_POINT('Ctrl Pts',(-1.45260539265259,3.6550821937918,-8.22000743827012));
#38079=CARTESIAN_POINT('Ctrl Pts',(-1.3743127963151,5.95323704169039,-6.41925818630909));
#38080=CARTESIAN_POINT('Ctrl Pts',(-1.33516649814636,6.82239825464977,-5.30055113218915));
#38081=CARTESIAN_POINT('Ctrl Pts',(-11.7398335018536,4.84822929958311,-6.80323369131649));
#38082=CARTESIAN_POINT('Ctrl Pts',(-11.7006872036849,5.96379383235061,-6.00824223596748));
#38083=CARTESIAN_POINT('Ctrl Pts',(-11.6223946073474,7.79543266737381,-3.85993105185963));
#38084=CARTESIAN_POINT('Ctrl Pts',(-11.5049557128412,8.69396726206043,0.280394411340654));
#38085=CARTESIAN_POINT('Ctrl Pts',(-11.3875168183349,7.53075696430187,4.35320836797643));
#38086=CARTESIAN_POINT('Ctrl Pts',(-11.2700779238287,4.58160321270218,7.39415014262294));
#38087=CARTESIAN_POINT('Ctrl Pts',(-11.1526390293225,0.545923703805717,
8.68130953564814));
#38088=CARTESIAN_POINT('Ctrl Pts',(-11.0352001348162,-3.61922588497217,
7.90981255230121));
#38089=CARTESIAN_POINT('Ctrl Pts',(-10.91776124031,-6.92606972083871,5.26242918861808));
#38090=CARTESIAN_POINT('Ctrl Pts',(-10.8003223458038,-8.5903884078789,1.36708690845965));
#38091=CARTESIAN_POINT('Ctrl Pts',(-10.6828834512975,-8.21748530084544,
-2.85247835334975));
#38092=CARTESIAN_POINT('Ctrl Pts',(-10.5654445567913,-5.89579554376979,
-6.39556638001792));
#38093=CARTESIAN_POINT('Ctrl Pts',(-10.4480056622851,-2.17591039922154,
-8.42194214584341));
#38094=CARTESIAN_POINT('Ctrl Pts',(-10.3305667677788,2.05999454897933,-8.45104165332889));
#38095=CARTESIAN_POINT('Ctrl Pts',(-10.2131278732726,5.80736925177168,-6.47596719630671));
#38096=CARTESIAN_POINT('Ctrl Pts',(-10.0956889787664,8.1775190775919,-2.9651084812346));
#38097=CARTESIAN_POINT('Ctrl Pts',(-9.97825008426016,8.60836006298699,1.248929123778));
#38098=CARTESIAN_POINT('Ctrl Pts',(-9.8608111897539,6.99771771880634,5.16678177385116));
#38099=CARTESIAN_POINT('Ctrl Pts',(-9.74337229524769,3.72755789195307,7.85932560877514));
#38100=CARTESIAN_POINT('Ctrl Pts',(-9.62593340074144,-0.426596939130836,
8.6880206104666));
#38101=CARTESIAN_POINT('Ctrl Pts',(-9.50849450623522,-4.47958377350399,
7.45634066956625));
#38102=CARTESIAN_POINT('Ctrl Pts',(-9.39105561172899,-7.47023172921315,
4.456380248742));
#38103=CARTESIAN_POINT('Ctrl Pts',(-9.27361671722275,-8.68930491314286,
0.399583688947602));
#38104=CARTESIAN_POINT('Ctrl Pts',(-9.15617782271653,-7.84769859947314,
-3.75197463857764));
#38105=CARTESIAN_POINT('Ctrl Pts',(-9.03873892821029,-5.14500077505786,
-7.01374750226396));
#38106=CARTESIAN_POINT('Ctrl Pts',(-8.92130003370406,-1.22215959988252,
-8.61220139743023));
#38107=CARTESIAN_POINT('Ctrl Pts',(-8.80386113919782,2.99051824872198,-8.16826099016765));
#38108=CARTESIAN_POINT('Ctrl Pts',(-8.6864222446916,6.49399096478861,-5.78720730126397));
#38109=CARTESIAN_POINT('Ctrl Pts',(-8.56898335018535,8.45740562409074,-2.03371018299995));
#38110=CARTESIAN_POINT('Ctrl Pts',(-8.45154445567914,8.41513599135171,2.20208384169883));
#38111=CARTESIAN_POINT('Ctrl Pts',(-8.33410556117289,6.37720636269711,5.91565093682343));
#38112=CARTESIAN_POINT('Ctrl Pts',(-8.21666666666667,2.82691429131802,8.22631403414417));
#38113=CARTESIAN_POINT('Ctrl Pts',(-8.09922777216043,-1.39378403004486,
8.58609649819838));
#38114=CARTESIAN_POINT('Ctrl Pts',(-7.9817888776542,-5.28394473032056,6.90967546891433));
#38115=CARTESIAN_POINT('Ctrl Pts',(-7.86434998314797,-7.92101134753324,
3.59461628425654));
#38116=CARTESIAN_POINT('Ctrl Pts',(-7.74691108864174,-8.67960024439589,
-0.572910635506885));
#38117=CARTESIAN_POINT('Ctrl Pts',(-7.6294721941355,-7.37981111788649,-4.60457108351182));
#38118=CARTESIAN_POINT('Ctrl Pts',(-7.51203329962927,-4.32989058048619,
-7.54425175612604));
#38119=CARTESIAN_POINT('Ctrl Pts',(-7.39459440512304,-0.253131091576217,
-8.69480371539643));
#38120=CARTESIAN_POINT('Ctrl Pts',(-7.2771555106168,3.88365875141243,-7.78337212918486));
#38121=CARTESIAN_POINT('Ctrl Pts',(-7.15971661611057,7.09943407770776,-5.02610413492158));
#38122=CARTESIAN_POINT('Ctrl Pts',(-7.04227772160433,8.63156975788372,-1.07688927637946));
#38123=CARTESIAN_POINT('Ctrl Pts',(-6.92483882709811,8.11671790446888,3.12771121717918));
#38124=CARTESIAN_POINT('Ctrl Pts',(-6.80739993259187,5.67697627663657,6.59057109462445));
#38125=CARTESIAN_POINT('Ctrl Pts',(-6.68996103808565,1.89093264433377,8.49046881705523));
#38126=CARTESIAN_POINT('Ctrl Pts',(-6.5725221435794,-2.34354802299109,8.3768412699972));
#38127=CARTESIAN_POINT('Ctrl Pts',(-6.45508324907318,-6.02225335373217,
6.27663536795438));
#38128=CARTESIAN_POINT('Ctrl Pts',(-6.33764435456695,-8.27277379053132,
2.68791756002525));
#38129=CARTESIAN_POINT('Ctrl Pts',(-6.22020546006071,-8.56139560489652,
-1.53824324970157));
#38130=CARTESIAN_POINT('Ctrl Pts',(-6.10276656555449,-6.81967177357477,
-5.39960775422637));
#38131=CARTESIAN_POINT('Ctrl Pts',(-5.98532767104824,-3.46065427548533,
-7.98044854531116));
#38132=CARTESIAN_POINT('Ctrl Pts',(-5.86788877654203,0.719061700249613,
-8.66871601046131));
#38133=CARTESIAN_POINT('Ctrl Pts',(-5.75044988203577,4.72825129693874,-7.30118666189211));
#38134=CARTESIAN_POINT('Ctrl Pts',(-5.63301098752956,7.61613020136608,-4.20217179023341));
#38135=CARTESIAN_POINT('Ctrl Pts',(-5.51557209302332,8.69783432951228,-0.106606637467579));
#38136=CARTESIAN_POINT('Ctrl Pts',(-5.39813319851709,7.71683619825904,4.01424041233612));
#38137=CARTESIAN_POINT('Ctrl Pts',(-5.28069430401086,4.90578073795857,7.18310534169375));
#38138=CARTESIAN_POINT('Ctrl Pts',(-5.16325540950462,0.931313257039131,
8.64848788032087));
#38139=CARTESIAN_POINT('Ctrl Pts',(-5.04581651499839,-3.26401632434385,
8.06287073152049));
#38140=CARTESIAN_POINT('Ctrl Pts',(-4.92837762049216,-6.68528036344698,
5.56513373252692));
#38141=CARTESIAN_POINT('Ctrl Pts',(-4.81093872598592,-8.52112182630912,
1.74761832789114));
#38142=CARTESIAN_POINT('Ctrl Pts',(-4.6934998314797,-8.33616862030953,-2.48434694287691));
#38143=CARTESIAN_POINT('Ctrl Pts',(-4.57606093697345,-6.17428262892098,
-6.12714623760273));
#38144=CARTESIAN_POINT('Ctrl Pts',(-4.45862204246723,-2.54815781137567,
-8.31688516015095));
#38145=CARTESIAN_POINT('Ctrl Pts',(-4.34118314796099,1.68226580928467,-8.53426439394464));
#38146=CARTESIAN_POINT('Ctrl Pts',(-4.22374425345477,5.51373799506711,-6.72773218256439));
#38147=CARTESIAN_POINT('Ctrl Pts',(-4.10630535894853,8.03762033853134,-3.3257098930997));
#38148=CARTESIAN_POINT('Ctrl Pts',(-3.9888664644423,8.65537099382864,0.865008645433196));
#38149=CARTESIAN_POINT('Ctrl Pts',(-3.87142756993607,7.22048962306834,4.85058930481876));
#38150=CARTESIAN_POINT('Ctrl Pts',(-3.75398867542984,4.07326013198663,7.68584666083514));
#38151=CARTESIAN_POINT('Ctrl Pts',(-3.6365497809236,-0.0399480784137633,
8.69839589516784));
#38152=CARTESIAN_POINT('Ctrl Pts',(-3.51911088641737,-4.1436825546629,7.64810969427759));
#38153=CARTESIAN_POINT('Ctrl Pts',(-3.40167199191113,-7.26473754010695,
4.7840647401377));
#38154=CARTESIAN_POINT('Ctrl Pts',(-3.28423309740491,-8.66295096673114,
0.785472866736996));
#38155=CARTESIAN_POINT('Ctrl Pts',(-3.16679420289867,-8.00673474808114,
-3.39939487798645));
#38156=CARTESIAN_POINT('Ctrl Pts',(-3.04935530839244,-5.45171143488453,
-6.77809188499583));
#38157=CARTESIAN_POINT('Ctrl Pts',(-2.9319164138862,-1.60380788220162,-8.54935595277434));
#38158=CARTESIAN_POINT('Ctrl Pts',(-2.81447751937998,2.62444056588667,-8.29312958333569));
#38159=CARTESIAN_POINT('Ctrl Pts',(-2.69703862487374,6.23029994447327,-6.07017720960104));
#38160=CARTESIAN_POINT('Ctrl Pts',(-2.57959973036751,8.35863536131798,-2.4076747007536));
#38161=CARTESIAN_POINT('Ctrl Pts',(-2.46216083586128,8.50471107882439,1.82581078951133));
#38162=CARTESIAN_POINT('Ctrl Pts',(-2.34472194135504,6.63388178670012,5.62630312507595));
#38163=CARTESIAN_POINT('Ctrl Pts',(-2.22728304684882,3.1898234291443,8.09251035938923));
#38164=CARTESIAN_POINT('Ctrl Pts',(-2.10984415234258,-1.01071395196248,
8.63956925551327));
#38165=CARTESIAN_POINT('Ctrl Pts',(-1.99240525783635,-4.97154267613221,
7.13774237154401));
#38166=CARTESIAN_POINT('Ctrl Pts',(-1.87496636333012,-7.75339651687287,
3.94319325815235));
#38167=CARTESIAN_POINT('Ctrl Pts',(-1.75752746882388,-8.69645836556818,
-0.186493538899628));
#38168=CARTESIAN_POINT('Ctrl Pts',(-1.64008857431765,-7.57727101680884,
-4.27194431940803));
#38169=CARTESIAN_POINT('Ctrl Pts',(-1.52264967981142,-4.66087445293086,
-7.34431568523695));
#38170=CARTESIAN_POINT('Ctrl Pts',(-1.40521078530519,-0.639641264381448,
-8.67493785756361));
#38171=CARTESIAN_POINT('Ctrl Pts',(-1.28777189079895,3.53429673556765,-7.94836994493994));
#38172=CARTESIAN_POINT('Ctrl Pts',(-1.20947929446147,5.75650700228966,-6.20712806162696));
#38173=CARTESIAN_POINT('Ctrl Pts',(-1.17033299629272,6.59694600605871,-5.12538968207745));
#38174=CARTESIAN_POINT('Ctrl Pts',(-11.575,4.68253987355595,-6.57073151046051));
#38175=CARTESIAN_POINT('Ctrl Pts',(-11.5358537018313,5.75997971466614,-5.80290908318214));
#38176=CARTESIAN_POINT('Ctrl Pts',(-11.4575611054938,7.52902184303394,-3.72801696096832));
#38177=CARTESIAN_POINT('Ctrl Pts',(-11.3401222109875,8.39684879745447,0.270811863526706));
#38178=CARTESIAN_POINT('Ctrl Pts',(-11.2226833164813,7.27339149706363,4.20443640376082));
#38179=CARTESIAN_POINT('Ctrl Pts',(-11.1052444219751,4.42502579862193,7.14145324703773));
#38180=CARTESIAN_POINT('Ctrl Pts',(-10.9878055274688,0.527266627263149,
8.38462365194841));
#38181=CARTESIAN_POINT('Ctrl Pts',(-10.8703666329626,-3.49553795222623,
7.63949276732611));
#38182=CARTESIAN_POINT('Ctrl Pts',(-10.7529277384564,-6.68936958853091,
5.08258437974203));
#38183=CARTESIAN_POINT('Ctrl Pts',(-10.6354888439501,-8.29680977603194,
1.32036637789162));
#38184=CARTESIAN_POINT('Ctrl Pts',(-10.5180499494439,-7.93665072418858,
-2.7549942056503));
#38185=CARTESIAN_POINT('Ctrl Pts',(-10.4006110549377,-5.69430528428376,
-6.17699632956363));
#38186=CARTESIAN_POINT('Ctrl Pts',(-10.2831721604314,-2.10154812737837,
-8.1341202063368));
#38187=CARTESIAN_POINT('Ctrl Pts',(-10.1657332659252,1.98959372976295,-8.16222523101317));
#38188=CARTESIAN_POINT('Ctrl Pts',(-10.048294371419,5.60890098251375,-6.25464942822609));
#38189=CARTESIAN_POINT('Ctrl Pts',(-9.93085547691274,7.89805035642209,-2.86377517127619));
#38190=CARTESIAN_POINT('Ctrl Pts',(-9.8134165824065,8.31416724541664,1.20624666449639));
#38191=CARTESIAN_POINT('Ctrl Pts',(-9.69597768790028,6.75856899858617,4.99020573884583));
#38192=CARTESIAN_POINT('Ctrl Pts',(-9.57853879339404,3.60016768628482,7.59073122748412));
#38193=CARTESIAN_POINT('Ctrl Pts',(-9.46109989888781,-0.412017884052814,
8.3911053741381));
#38194=CARTESIAN_POINT('Ctrl Pts',(-9.34366100438158,-4.32649289879303,
7.20151839746173));
#38195=CARTESIAN_POINT('Ctrl Pts',(-9.22622210987535,-7.21493472673645,
4.30408236018371));
#38196=CARTESIAN_POINT('Ctrl Pts',(-9.10878321536912,-8.39234578545526,
0.385927818323404));
#38197=CARTESIAN_POINT('Ctrl Pts',(-8.99134432086288,-7.57950157407817,
-3.62374998460184));
#38198=CARTESIAN_POINT('Ctrl Pts',(-8.87390542635665,-4.96916911103115,
-6.77405096026056));
#38199=CARTESIAN_POINT('Ctrl Pts',(-8.75646653185041,-1.18039199564904,
-8.31787730131265));
#38200=CARTESIAN_POINT('Ctrl Pts',(-8.63902763734419,2.88831655372436,-7.88910866640744));
#38201=CARTESIAN_POINT('Ctrl Pts',(-8.52158874283795,6.27205722999723,-5.5894280716122));
#38202=CARTESIAN_POINT('Ctrl Pts',(-8.40414984833172,8.16837171151259,-1.96420763844087));
#38203=CARTESIAN_POINT('Ctrl Pts',(-8.28671095382549,8.12754665384501,2.12682708603627));
#38204=CARTESIAN_POINT('Ctrl Pts',(-8.16927205931926,6.15926377034014,5.71348211440747));
#38205=CARTESIAN_POINT('Ctrl Pts',(-8.05183316481303,2.73030380171169,7.94517773336033));
#38206=CARTESIAN_POINT('Ctrl Pts',(-7.93439427030679,-1.34615111879544,
8.29266454341796));
#38207=CARTESIAN_POINT('Ctrl Pts',(-7.81695537580056,-5.1033646225271,6.67353561418904));
#38208=CARTESIAN_POINT('Ctrl Pts',(-7.69951648129434,-7.650308840983,3.47176939065404));
#38209=CARTESIAN_POINT('Ctrl Pts',(-7.58207758678809,-8.38297277614415,
-0.553331273951084));
#38210=CARTESIAN_POINT('Ctrl Pts',(-7.46463869228187,-7.12760426199033,
-4.44720873681053));
#38211=CARTESIAN_POINT('Ctrl Pts',(-7.34719979777563,-4.18191550738002,
-7.28642510106571));
#38212=CARTESIAN_POINT('Ctrl Pts',(-7.2297609032694,-0.244480274405397,
-8.39765666479245));
#38213=CARTESIAN_POINT('Ctrl Pts',(-7.11232200876316,3.75093376056635,-7.51737347669715));
#38214=CARTESIAN_POINT('Ctrl Pts',(-6.99488311425694,6.85680917596183,-4.85433579274776));
#38215=CARTESIAN_POINT('Ctrl Pts',(-6.8774442197507,8.33658374329481,-1.04008632109978));
#38216=CARTESIAN_POINT('Ctrl Pts',(-6.76000532524447,7.83932707831064,3.02082091881856));
#38217=CARTESIAN_POINT('Ctrl Pts',(-6.64256643073823,5.48296421930119,6.36533671019601));
#38218=CARTESIAN_POINT('Ctrl Pts',(-6.52512753623201,1.82630955719499,8.20030496174408));
#38219=CARTESIAN_POINT('Ctrl Pts',(-6.40768864172577,-2.26345669421878,
8.09056066399));
#38220=CARTESIAN_POINT('Ctrl Pts',(-6.29024974721954,-5.81644136755901,
6.06212981402202));
#38221=CARTESIAN_POINT('Ctrl Pts',(-6.17281085271331,-7.99004971617214,
2.59605731781944));
#38222=CARTESIAN_POINT('Ctrl Pts',(-6.05537195820707,-8.26880780920608,
-1.48567340917131));
#38223=CARTESIAN_POINT('Ctrl Pts',(-5.93793306370085,-6.58660781722385,
-5.21507483420824));
#38224=CARTESIAN_POINT('Ctrl Pts',(-5.8204941691946,-3.34238556640572,-7.70771475794147));
#38225=CARTESIAN_POINT('Ctrl Pts',(-5.70305527468838,0.694487590192009,
-8.37246051357519));
#38226=CARTESIAN_POINT('Ctrl Pts',(-5.58561638018214,4.56666214859352,-7.0516668160733));
#38227=CARTESIAN_POINT('Ctrl Pts',(-5.46817748567591,7.35584708280132,-4.05856153812523));
#38228=CARTESIAN_POINT('Ctrl Pts',(-5.35073859116968,8.40058370692718,-0.102963329471767));
#38229=CARTESIAN_POINT('Ctrl Pts',(-5.23329969666345,7.45311142753807,3.87705276118435));
#38230=CARTESIAN_POINT('Ctrl Pts',(-5.11586080215721,4.73812447740229,6.93762095396888));
#38231=CARTESIAN_POINT('Ctrl Pts',(-4.99842190765099,0.89948539794352,8.35292368474611));
#38232=CARTESIAN_POINT('Ctrl Pts',(-4.88098301314475,-3.15246776549777,
7.7873201457114));
#38233=CARTESIAN_POINT('Ctrl Pts',(-4.76354411863852,-6.45680926651568,
5.37494392158168));
#38234=CARTESIAN_POINT('Ctrl Pts',(-4.64610522413228,-8.22991039688474,
1.6878930426849));
#38235=CARTESIAN_POINT('Ctrl Pts',(-4.52866632962606,-8.05127801208613,
-2.39944377646666));
#38236=CARTESIAN_POINT('Ctrl Pts',(-4.41122743511982,-5.96327500496155,
-5.91774951138349));
#38237=CARTESIAN_POINT('Ctrl Pts',(-4.29378854061358,-2.46107389287582,
-8.03265356891045));
#38238=CARTESIAN_POINT('Ctrl Pts',(-4.17634964610736,1.62477396243877,-8.24260381404624));
#38239=CARTESIAN_POINT('Ctrl Pts',(-4.05891075160112,5.32530464606164,-6.49781028429742));
#38240=CARTESIAN_POINT('Ctrl Pts',(-3.94147185709489,7.76293269109889,-3.21205294140231));
#38241=CARTESIAN_POINT('Ctrl Pts',(-3.82403296258866,8.35957156616068,0.835446762709816));
#38242=CARTESIAN_POINT('Ctrl Pts',(-3.70659406808243,6.97372761835372,4.68481922503354));
#38243=CARTESIAN_POINT('Ctrl Pts',(-3.58915517357619,3.93405546743286,7.42318096516021));
#38244=CARTESIAN_POINT('Ctrl Pts',(-3.47171627906997,-0.0385828430310631,
8.40112608093868));
#38245=CARTESIAN_POINT('Ctrl Pts',(-3.35427738456373,-4.00207118653311,
7.38673366869508));
#38246=CARTESIAN_POINT('Ctrl Pts',(-3.2368384900575,-7.01646335196947,4.620568153675));
#38247=CARTESIAN_POINT('Ctrl Pts',(-3.11939959555127,-8.36689249162919,
0.758629138767949));
#38248=CARTESIAN_POINT('Ctrl Pts',(-3.00196070104503,-7.73310262328138,
-3.28321972384891));
#38249=CARTESIAN_POINT('Ctrl Pts',(-2.8845218065388,-5.26539785879409,-6.54644893154043));
#38250=CARTESIAN_POINT('Ctrl Pts',(-2.76708291203257,-1.54899735426666,
-8.25717961514961));
#38251=CARTESIAN_POINT('Ctrl Pts',(-2.64964401752634,2.53474966553227,-8.00970984476226));
#38252=CARTESIAN_POINT('Ctrl Pts',(-2.5322051230201,6.01737791500869,-5.86272741389347));
#38253=CARTESIAN_POINT('Ctrl Pts',(-2.41476622851387,8.07297694670747,-2.3253918270326));
#38254=CARTESIAN_POINT('Ctrl Pts',(-2.29732733400764,8.21406049072235,1.76341325774147));
#38255=CARTESIAN_POINT('Ctrl Pts',(-2.17988843950141,6.4071672487419,5.43402283512993));
#38256=CARTESIAN_POINT('Ctrl Pts',(-2.06244954499518,3.08081043069796,7.81594683202442));
#38257=CARTESIAN_POINT('Ctrl Pts',(-1.94501065048894,-0.976172554633629,
8.34430985612986));
#38258=CARTESIAN_POINT('Ctrl Pts',(-1.82757175598271,-4.80163898520143,
6.89380827445569));
#38259=CARTESIAN_POINT('Ctrl Pts',(-1.71013286147648,-7.4884222882917,3.80843366092916));
#38260=CARTESIAN_POINT('Ctrl Pts',(-1.59269396697024,-8.39925476688854,
-0.18012007644382));
#38261=CARTESIAN_POINT('Ctrl Pts',(-1.47525507246401,-7.31831592041203,
-4.12594957399375));
#38262=CARTESIAN_POINT('Ctrl Pts',(-1.35781617795778,-4.50158792476329,
-7.09332189446186));
#38263=CARTESIAN_POINT('Ctrl Pts',(-1.24037728345155,-0.617781367208725,
-8.37846972752598));
#38264=CARTESIAN_POINT('Ctrl Pts',(-1.12293838894532,3.41351127734351,-7.67673245160975));
#38265=CARTESIAN_POINT('Ctrl Pts',(-1.04464579260783,5.55977696288894,-5.99499793694482));
#38266=CARTESIAN_POINT('Ctrl Pts',(-1.00549949443908,6.37149375746765,-4.95022823196575));
#38267=CARTESIAN_POINT('',(-1.5,7.04785050324084,-5.47571258230085));
#38268=CARTESIAN_POINT('Ctrl Pts',(-1.5,-7.40071554151276,-3.21429017473183));
#38269=CARTESIAN_POINT('Ctrl Pts',(-1.5,-7.32607552716124,-3.41408847491103));
#38270=CARTESIAN_POINT('Ctrl Pts',(-1.5,-7.24365422857139,-3.61052987409804));
#38271=CARTESIAN_POINT('Ctrl Pts',(-1.5,-7.1536381226817,-3.80314116313213));
#38272=CARTESIAN_POINT('Ctrl Pts',(-1.5,-7.12529565119459,-3.86378675442481));
#38273=CARTESIAN_POINT('Ctrl Pts',(-1.5,-7.09619986523178,-3.92405263504233));
#38274=CARTESIAN_POINT('Ctrl Pts',(-1.5,-7.06635552234977,-3.98392396459837));
#38275=CARTESIAN_POINT('Ctrl Pts',(-1.5,-6.97243139747263,-4.17234701870998));
#38276=CARTESIAN_POINT('Ctrl Pts',(-1.5,-6.87109710954449,-4.35686339452859));
#38277=CARTESIAN_POINT('Ctrl Pts',(-1.5,-6.76274048915299,-4.53715619452641));
#38278=CARTESIAN_POINT('Ctrl Pts',(-1.5,-6.65334098717867,-4.71918422805175));
#38279=CARTESIAN_POINT('Ctrl Pts',(-1.5,-6.53678300025226,-4.89690755496705));
#38280=CARTESIAN_POINT('Ctrl Pts',(-1.5,-6.41341608194796,-5.06998046755394));
#38281=CARTESIAN_POINT('Ctrl Pts',(-1.5,-6.28977894266464,-5.24343247635658));
#38282=CARTESIAN_POINT('Ctrl Pts',(-1.5,-6.15930261540002,-5.41221423931513));
#38283=CARTESIAN_POINT('Ctrl Pts',(-1.5,-6.0222949455953,-5.5759497740738));
#38284=CARTESIAN_POINT('Ctrl Pts',(-1.5,-5.96511117533728,-5.64428912482739));
#38285=CARTESIAN_POINT('Ctrl Pts',(-1.5,-5.90678913255776,-5.71174902319245));
#38286=CARTESIAN_POINT('Ctrl Pts',(-1.5,-5.84734919270319,-5.77830033033274));
#38287=CARTESIAN_POINT('Ctrl Pts',(-1.5,-5.82312043264619,-5.80542780818899));
#38288=CARTESIAN_POINT('Ctrl Pts',(-1.5,-5.79870591888853,-5.83240430838032));
#38289=CARTESIAN_POINT('Ctrl Pts',(-1.5,-5.77410697966433,-5.85922780040854));
#38290=CARTESIAN_POINT('Ctrl Pts',(-1.5,-5.75257308437455,-5.88270906776637));
#38291=CARTESIAN_POINT('Ctrl Pts',(-1.5,-5.73089516063029,-5.90607586915347));
#38292=CARTESIAN_POINT('Ctrl Pts',(-1.5,-5.70909277099336,-5.92930716662182));
#38293=CARTESIAN_POINT('Ctrl Pts',(-1.5,-5.56150733846096,-6.08656520770133));
#38294=CARTESIAN_POINT('Ctrl Pts',(-1.5,-5.40806704913402,-6.23778842012323));
#38295=CARTESIAN_POINT('Ctrl Pts',(-1.5,-5.24917010701384,-6.38265417970832));
#38296=CARTESIAN_POINT('Ctrl Pts',(-1.5,-5.08916305305425,-6.52853202418754));
#38297=CARTESIAN_POINT('Ctrl Pts',(-1.5,-4.92362244634448,-6.66796384769363));
#38298=CARTESIAN_POINT('Ctrl Pts',(-1.5,-4.75290905048751,-6.80059432958983));
#38299=CARTESIAN_POINT('Ctrl Pts',(-1.5,-4.65550778899749,-6.87626722089323));
#38300=CARTESIAN_POINT('Ctrl Pts',(-1.5,-4.55642181271268,-6.94972553712658));
#38301=CARTESIAN_POINT('Ctrl Pts',(-1.5,-4.45571226131071,-7.02089844525531));
#38302=CARTESIAN_POINT('Ctrl Pts',(-1.5,-4.27985527394039,-7.145179141889));
#38303=CARTESIAN_POINT('Ctrl Pts',(-1.5,-4.09904947818624,-7.26249377733021));
#38304=CARTESIAN_POINT('Ctrl Pts',(-1.5,-3.91376263334626,-7.37270325078949));
#38305=CARTESIAN_POINT('Ctrl Pts',(-1.5,-3.78859158583618,-7.44715556957309));
#38306=CARTESIAN_POINT('Ctrl Pts',(-1.5,-3.66137477543102,-7.51836446454134));
#38307=CARTESIAN_POINT('Ctrl Pts',(-1.5,-3.53224920673504,-7.58627572011563));
#38308=CARTESIAN_POINT('Ctrl Pts',(-1.5,-3.41926433412606,-7.64569806874313));
#38309=CARTESIAN_POINT('Ctrl Pts',(-1.5,-3.30481794856632,-7.70259554193464));
#38310=CARTESIAN_POINT('Ctrl Pts',(-1.5,-3.18899907397327,-7.75692565137345));
#38311=CARTESIAN_POINT('Ctrl Pts',(-1.5,-3.15879244923969,-7.77109544220692));
#38312=CARTESIAN_POINT('Ctrl Pts',(-1.5,-3.12848823906593,-7.78509241552022));
#38313=CARTESIAN_POINT('Ctrl Pts',(-1.5,-3.09811472952744,-7.79890379709708));
#38314=CARTESIAN_POINT('Ctrl Pts',(-1.5,-2.8992287670567,-7.88934082461551));
#38315=CARTESIAN_POINT('Ctrl Pts',(-1.5,-2.69717640931447,-7.97191903960201));
#38316=CARTESIAN_POINT('Ctrl Pts',(-1.5,-2.49247199354083,-8.04655431134645));
#38317=CARTESIAN_POINT('Ctrl Pts',(-1.5,-2.2863262339712,-8.1217150973329));
#38318=CARTESIAN_POINT('Ctrl Pts',(-1.5,-2.07749034379047,-8.18882100549067));
#38319=CARTESIAN_POINT('Ctrl Pts',(-1.5,-1.8664568012609,-8.24774400472739));
#38320=CARTESIAN_POINT('Ctrl Pts',(-1.5,-1.65568015538806,-8.30659527545438));
#38321=CARTESIAN_POINT('Ctrl Pts',(-1.5,-1.44271056686449,-8.35728381421289));
#38322=CARTESIAN_POINT('Ctrl Pts',(-1.5,-1.22801543305964,-8.39963592793665));
#38323=CARTESIAN_POINT('Ctrl Pts',(-1.5,-1.02879612386665,-8.43893518306825));
#38324=CARTESIAN_POINT('Ctrl Pts',(-1.5,-0.82809043936243,-8.4710562447127));
#38325=CARTESIAN_POINT('Ctrl Pts',(-1.5,-0.626261042790105,-8.49582164860091));
#38326=CARTESIAN_POINT('Ctrl Pts',(-1.5,-0.450826239746891,-8.51734831333459));
#38327=CARTESIAN_POINT('Ctrl Pts',(-1.5,-0.274542073599355,-8.53331679425628));
#38328=CARTESIAN_POINT('Ctrl Pts',(-1.5,-0.0976585345107927,-8.54375388314286));
#38329=CARTESIAN_POINT('Ctrl Pts',(-1.5,-0.0616353375598041,-8.54587944728802));
#38330=CARTESIAN_POINT('Ctrl Pts',(-1.5,-0.0255872814160311,-8.54777552216579));
#38331=CARTESIAN_POINT('Ctrl Pts',(-1.5,0.0104835191461953,-8.54944222208194));
#38332=CARTESIAN_POINT('Ctrl Pts',(-1.5,0.0356559460320415,-8.55060534796564));
#38333=CARTESIAN_POINT('Ctrl Pts',(-1.5,0.0608395666875181,-8.55165672685359));
#38334=CARTESIAN_POINT('Ctrl Pts',(-1.5,0.0860189798068464,-8.55259596649835));
#38335=CARTESIAN_POINT('Ctrl Pts',(-1.5,0.304647650635756,-8.56075122866235));
#38336=CARTESIAN_POINT('Ctrl Pts',(-1.5,0.523231328293199,-8.56046971217016));
#38337=CARTESIAN_POINT('Ctrl Pts',(-1.5,0.741283405020929,-8.5519315510966));
#38338=CARTESIAN_POINT('Ctrl Pts',(-1.5,0.962291191374389,-8.54327765471223));
#38339=CARTESIAN_POINT('Ctrl Pts',(-1.5,1.18275348637413,-8.52614180962386));
#38340=CARTESIAN_POINT('Ctrl Pts',(-1.5,1.40217760172751,-8.50066002463597));
#38341=CARTESIAN_POINT('Ctrl Pts',(-1.5,1.62328838446544,-8.47498236648452));
#38342=CARTESIAN_POINT('Ctrl Pts',(-1.5,1.84334564184632,-8.44082997916866));
#38343=CARTESIAN_POINT('Ctrl Pts',(-1.5,2.0618494910781,-8.39828963846045));
#38344=CARTESIAN_POINT('Ctrl Pts',(-1.5,2.27958312201272,-8.35589925094023));
#38345=CARTESIAN_POINT('Ctrl Pts',(-1.5,2.49577496126564,-8.30517986494593));
#38346=CARTESIAN_POINT('Ctrl Pts',(-1.5,2.70992438663794,-8.24616614721805));
#38347=CARTESIAN_POINT('Ctrl Pts',(-1.5,2.85086308604455,-8.20732730088794));
#38348=CARTESIAN_POINT('Ctrl Pts',(-1.5,2.99091699653584,-8.16489481765947));
#38349=CARTESIAN_POINT('Ctrl Pts',(-1.5,3.12993979573812,-8.11886663092679));
#38350=CARTESIAN_POINT('Ctrl Pts',(-1.5,3.17554939098335,-8.10376603606901));
#38351=CARTESIAN_POINT('Ctrl Pts',(-1.5,3.22104797579745,-8.0882783538033));
#38352=CARTESIAN_POINT('Ctrl Pts',(-1.5,3.266430287064,-8.07240329011238));
#38353=CARTESIAN_POINT('Ctrl Pts',(-1.5,3.2928090607661,-8.06317580255341));
#38354=CARTESIAN_POINT('Ctrl Pts',(-1.5,3.31915086873423,-8.05381659336008));
#38355=CARTESIAN_POINT('Ctrl Pts',(-1.5,3.3454470923227,-8.04432832850057));
#38356=CARTESIAN_POINT('Ctrl Pts',(-1.5,3.41180769954115,-8.0203839390939));
#38357=CARTESIAN_POINT('Ctrl Pts',(-1.5,3.47784485409642,-7.99562983843644));
#38358=CARTESIAN_POINT('Ctrl Pts',(-1.5,3.54354309403428,-7.97006958073044));
#38359=CARTESIAN_POINT('Ctrl Pts',(-1.5,3.75098753387345,-7.88936219272456));
#38360=CARTESIAN_POINT('Ctrl Pts',(-1.5,3.95505373021087,-7.80062138510352));
#38361=CARTESIAN_POINT('Ctrl Pts',(-1.5,4.15538780312082,-7.70421697836692));
#38362=CARTESIAN_POINT('Ctrl Pts',(-1.5,4.35776901904387,-7.60682744910566));
#38363=CARTESIAN_POINT('Ctrl Pts',(-1.5,4.55634201706475,-7.50161663005502));
#38364=CARTESIAN_POINT('Ctrl Pts',(-1.5,4.75072757572629,-7.38891433258144));
#38365=CARTESIAN_POINT('Ctrl Pts',(-1.5,4.858921773029,-7.32618470033259));
#38366=CARTESIAN_POINT('Ctrl Pts',(-1.5,4.96581840178216,-7.26113332494834));
#38367=CARTESIAN_POINT('Ctrl Pts',(-1.5,5.07134916269885,-7.1938107550044));
#38368=CARTESIAN_POINT('Ctrl Pts',(-1.5,5.1522016547485,-7.14223150451977));
#38369=CARTESIAN_POINT('Ctrl Pts',(-1.5,5.23225235935691,-7.08931899950226));
#38370=CARTESIAN_POINT('Ctrl Pts',(-1.5,5.31146952438616,-7.03509430816655));
#38371=CARTESIAN_POINT('Ctrl Pts',(-1.5,5.34027476981638,-7.01537692063159));
#38372=CARTESIAN_POINT('Ctrl Pts',(-1.5,5.36897116188161,-6.99548498996351));
#38373=CARTESIAN_POINT('Ctrl Pts',(-1.5,5.39754124998948,-6.97543084519802));
#38374=CARTESIAN_POINT('Ctrl Pts',(-1.5,5.58374239728194,-6.84473104654129));
#38375=CARTESIAN_POINT('Ctrl Pts',(-1.5,5.76473134029108,-6.70704298605941));
#38376=CARTESIAN_POINT('Ctrl Pts',(-1.5,5.94013091598919,-6.56272128494992));
#38377=CARTESIAN_POINT('Ctrl Pts',(-1.5,6.11595427972063,-6.4180508839668));
#38378=CARTESIAN_POINT('Ctrl Pts',(-1.5,6.28616181452858,-6.26671438967896));
#38379=CARTESIAN_POINT('Ctrl Pts',(-1.5,6.45034955006475,-6.10902252251836));
#38380=CARTESIAN_POINT('Ctrl Pts',(-1.5,6.61343122693438,-5.95239295429102));
#38381=CARTESIAN_POINT('Ctrl Pts',(-1.5,6.77057447053939,-5.7894929424118));
#38382=CARTESIAN_POINT('Ctrl Pts',(-1.5,6.92135144632236,-5.62058700655496));
#38383=CARTESIAN_POINT('Ctrl Pts',(-1.5,6.96403155771474,-5.57277516976909));
#38384=CARTESIAN_POINT('Ctrl Pts',(-1.5,7.00620133181954,-5.5244818677487));
#38385=CARTESIAN_POINT('Ctrl Pts',(-1.5,7.04785050324084,-5.47571258230085));
#38386=CARTESIAN_POINT('Ctrl Pts',(-1.5,7.0478505032408,-5.4757125823009));
#38387=CARTESIAN_POINT('Ctrl Pts',(-1.53914629816874,6.14996708109109,-6.63138831099123));
#38388=CARTESIAN_POINT('Ctrl Pts',(-1.57829259633749,4.96291736655354,-7.56151662129575));
#38389=CARTESIAN_POINT('Ctrl Pts',(-1.61743889450623,3.62618772416099,-8.15595230745444));
#38390=CARTESIAN_POINT('Ctrl Pts',(-1.65658519267497,2.28945808176837,-8.75038799361316));
#38391=CARTESIAN_POINT('Ctrl Pts',(-1.69573149084372,0.803048511520739,
-9.00913105562603));
#38392=CARTESIAN_POINT('Ctrl Pts',(-1.73487778901246,-0.656170682026274,
-8.9015741114905));
#38393=CARTESIAN_POINT('Ctrl Pts',(-1.77402408718121,-2.11538987557327,
-8.79401716735496));
#38394=CARTESIAN_POINT('Ctrl Pts',(-1.81317038534995,-3.54741869241963,
-8.32016021707105));
#38395=CARTESIAN_POINT('Ctrl Pts',(-1.8523166835187,-4.7827220508989,-7.53617016583733));
#38396=CARTESIAN_POINT('Ctrl Pts',(-1.89146298168744,-6.01802540937814,
-6.75218011460362));
#38397=CARTESIAN_POINT('Ctrl Pts',(-1.93060927985618,-7.05660330949029,
-5.65805696242012));
#38398=CARTESIAN_POINT('Ctrl Pts',(-1.96975557802493,-7.77517298510053,
-4.38354649525749));
#38399=CARTESIAN_POINT('Ctrl Pts',(-2.00890187619367,-8.49374266071079,
-3.10903602809483));
#38400=CARTESIAN_POINT('Ctrl Pts',(-2.04804817436242,-8.89230411181913,
-1.65413824595303));
#38401=CARTESIAN_POINT('Ctrl Pts',(-2.08719447253116,-8.92366473922459,
-0.191363868813808));
#38402=CARTESIAN_POINT('Ctrl Pts',(-2.0889007065657,-8.92503162632062,-0.127607254679447));
#38403=CARTESIAN_POINT('Ctrl Pts',(-2.09060694060025,-8.92570092469794,
-0.0638356770061805));
#38404=CARTESIAN_POINT('Ctrl Pts',(-2.09231317463479,-8.92567592894044,
-6.35753767513903E-5));
#38405=CARTESIAN_POINT('Origin',(-1.5,8.,0.));
#38406=CARTESIAN_POINT('Origin',(-1.5,0.,0.));
#38407=CARTESIAN_POINT('',(-1.5,-8.,-9.79717439317883E-16));
#38408=CARTESIAN_POINT('Origin',(-1.5,0.,0.));
#38409=CARTESIAN_POINT('Origin',(10.,-4.,2.3094010767585));
#38410=CARTESIAN_POINT('',(5.,-4.,2.3094010767585));
#38411=CARTESIAN_POINT('',(10.,-4.,2.3094010767585));
#38412=CARTESIAN_POINT('',(5.,2.82820063659975E-16,4.61880215351701));
#38413=CARTESIAN_POINT('Origin',(10.,-4.,-2.3094010767585));
#38414=CARTESIAN_POINT('',(5.,-4.,-2.3094010767585));
#38415=CARTESIAN_POINT('',(10.,-4.,-2.3094010767585));
#38416=CARTESIAN_POINT('',(5.,-4.,2.3094010767585));
#38417=CARTESIAN_POINT('Origin',(10.,-1.11022302462516E-15,-4.61880215351701));
#38418=CARTESIAN_POINT('',(5.,-4.,-2.3094010767585));
#38419=CARTESIAN_POINT('Origin',(5.,0.,0.));
#38420=CARTESIAN_POINT('Origin',(2.,-2.3332655251948E-15,-12.7017059221718));
#38421=CARTESIAN_POINT('',(2.,2.75,-11.1139926819003));
#38422=CARTESIAN_POINT('Origin',(2.,-11.,-6.35085296108589));
#38423=CARTESIAN_POINT('',(2.,-8.25,-7.93856620135736));
#38424=CARTESIAN_POINT('Origin',(2.,-11.,6.35085296108588));
#38425=CARTESIAN_POINT('',(2.,-11.,3.17542648054294));
#38426=CARTESIAN_POINT('Origin',(2.,0.,0.));
#38427=CARTESIAN_POINT('',(2.,-12.5,-1.53080849893419E-15));
#38428=CARTESIAN_POINT('Origin',(2.,0.,0.));
#38429=CARTESIAN_POINT('Origin',(0.,12.5,0.));
#38430=CARTESIAN_POINT('',(0.,-12.5,-1.53080849893419E-15));
#38431=CARTESIAN_POINT('Origin',(0.,0.,0.));
#38432=CARTESIAN_POINT('',(0.,-8.,-9.79717439317883E-16));
#38433=CARTESIAN_POINT('Origin',(0.,0.,0.));
#38434=CARTESIAN_POINT('Origin',(1.,0.,0.));
#38435=CARTESIAN_POINT('',(1.,-12.5,-1.53080849893419E-15));
#38436=CARTESIAN_POINT('Origin',(-12.,8.5,0.));
#38437=CARTESIAN_POINT('',(-12.,-8.5,-1.04094977927525E-15));
#38438=CARTESIAN_POINT('Origin',(-12.,0.,0.));
#38439=CARTESIAN_POINT('Origin',(-11.75,0.,0.));
#38440=CARTESIAN_POINT('',(-11.75,-8.75,-1.07156594925393E-15));
#38441=CARTESIAN_POINT('Origin',(-6.5,0.,0.));
#38442=CARTESIAN_POINT('Origin',(-0.75,0.,0.));
#38443=CARTESIAN_POINT('',(-0.75,-8.,-9.79717439317883E-16));
#38444=CARTESIAN_POINT('',(0.,0.,0.));
#38445=CARTESIAN_POINT('',(0.,0.,0.));
#38446=CARTESIAN_POINT('',(0.,0.,0.));
#38447=CARTESIAN_POINT('',(0.,0.,0.));
#38448=CARTESIAN_POINT('',(0.,0.,0.));
#38449=CARTESIAN_POINT('',(0.,0.,0.));
#38450=CARTESIAN_POINT('',(0.,0.,0.));
#38451=CARTESIAN_POINT('',(1.,0.,0.));
#38452=CARTESIAN_POINT('',(130.8,0.,0.));
#38453=CARTESIAN_POINT('',(-7.,0.,0.));
#38454=CARTESIAN_POINT('',(39.4168707478613,0.,28.));
#38455=CARTESIAN_POINT('',(29.9063055849098,0.,24.9098300562505));
#38456=CARTESIAN_POINT('',(42.8422669657035,21.8912815091048,17.4577144520445));
#38457=CARTESIAN_POINT('',(33.331701802752,21.8912815091048,14.3675445082951));
#38458=CARTESIAN_POINT('',(50.539062401846,27.2979815410911,-6.2305861507768));
#38459=CARTESIAN_POINT('',(41.0284972388945,27.2979815410911,-9.32075609452628));
#38460=CARTESIAN_POINT('',(56.7114131068591,12.1487446952916,-25.2271283012677));
#38461=CARTESIAN_POINT('',(47.2008479439076,12.1487446952916,-28.3172982450172));
#38462=CARTESIAN_POINT('',(56.7114131068591,-12.1487446952916,-25.2271283012677));
#38463=CARTESIAN_POINT('',(47.2008479439076,-12.1487446952916,-28.3172982450172));
#38464=CARTESIAN_POINT('',(50.539062401846,-27.2979815410911,-6.23058615077678));
#38465=CARTESIAN_POINT('',(41.0284972388945,-27.2979815410911,-9.32075609452626));
#38466=CARTESIAN_POINT('',(42.8422669657035,-21.8912815091048,17.4577144520445));
#38467=CARTESIAN_POINT('',(33.331701802752,-21.8912815091048,14.3675445082951));
#38468=CARTESIAN_POINT('',(39.0040570794311,-2.22044604925031E-15,-3.09016994374947));
#38469=CARTESIAN_POINT('',(162.,45.,45.));
#38470=CARTESIAN_POINT('',(162.,-45.,45.));
#38471=CARTESIAN_POINT('',(162.,45.,-45.));
#38472=CARTESIAN_POINT('',(162.,-45.,-45.));
#38473=CARTESIAN_POINT('',(62.5,18.,-64.));
#38474=UNCERTAINTY_MEASURE_WITH_UNIT(LENGTH_MEASURE(0.01),#38508,
'DISTANCE_ACCURACY_VALUE',
'Maximum model space distance between geometric entities at asserted c
onnectivities');
#38475=UNCERTAINTY_MEASURE_WITH_UNIT(LENGTH_MEASURE(0.01),#38508,
'DISTANCE_ACCURACY_VALUE',
'Maximum model space distance between geometric entities at asserted c
onnectivities');
#38476=UNCERTAINTY_MEASURE_WITH_UNIT(LENGTH_MEASURE(0.01),#38508,
'DISTANCE_ACCURACY_VALUE',
'Maximum model space distance between geometric entities at asserted c
onnectivities');
#38477=UNCERTAINTY_MEASURE_WITH_UNIT(LENGTH_MEASURE(0.01),#38508,
'DISTANCE_ACCURACY_VALUE',
'Maximum model space distance between geometric entities at asserted c
onnectivities');
#38478=UNCERTAINTY_MEASURE_WITH_UNIT(LENGTH_MEASURE(0.01),#38508,
'DISTANCE_ACCURACY_VALUE',
'Maximum model space distance between geometric entities at asserted c
onnectivities');
#38479=UNCERTAINTY_MEASURE_WITH_UNIT(LENGTH_MEASURE(0.01),#38508,
'DISTANCE_ACCURACY_VALUE',
'Maximum model space distance between geometric entities at asserted c
onnectivities');
#38480=UNCERTAINTY_MEASURE_WITH_UNIT(LENGTH_MEASURE(0.01),#38508,
'DISTANCE_ACCURACY_VALUE',
'Maximum model space distance between geometric entities at asserted c
onnectivities');
#38481=UNCERTAINTY_MEASURE_WITH_UNIT(LENGTH_MEASURE(0.01),#38508,
'DISTANCE_ACCURACY_VALUE',
'Maximum model space distance between geometric entities at asserted c
onnectivities');
#38482=UNCERTAINTY_MEASURE_WITH_UNIT(LENGTH_MEASURE(0.01),#38508,
'DISTANCE_ACCURACY_VALUE',
'Maximum model space distance between geometric entities at asserted c
onnectivities');
#38483=UNCERTAINTY_MEASURE_WITH_UNIT(LENGTH_MEASURE(0.01),#38508,
'DISTANCE_ACCURACY_VALUE',
'Maximum model space distance between geometric entities at asserted c
onnectivities');
#38484=UNCERTAINTY_MEASURE_WITH_UNIT(LENGTH_MEASURE(0.01),#38508,
'DISTANCE_ACCURACY_VALUE',
'Maximum model space distance between geometric entities at asserted c
onnectivities');
#38485=UNCERTAINTY_MEASURE_WITH_UNIT(LENGTH_MEASURE(0.01),#38508,
'DISTANCE_ACCURACY_VALUE',
'Maximum model space distance between geometric entities at asserted c
onnectivities');
#38486=UNCERTAINTY_MEASURE_WITH_UNIT(LENGTH_MEASURE(0.01),#38508,
'DISTANCE_ACCURACY_VALUE',
'Maximum model space distance between geometric entities at asserted c
onnectivities');
#38487=UNCERTAINTY_MEASURE_WITH_UNIT(LENGTH_MEASURE(0.01),#38508,
'DISTANCE_ACCURACY_VALUE',
'Maximum model space distance between geometric entities at asserted c
onnectivities');
#38488=UNCERTAINTY_MEASURE_WITH_UNIT(LENGTH_MEASURE(0.01),#38508,
'DISTANCE_ACCURACY_VALUE',
'Maximum model space distance between geometric entities at asserted c
onnectivities');
#38489=UNCERTAINTY_MEASURE_WITH_UNIT(LENGTH_MEASURE(0.01),#38508,
'DISTANCE_ACCURACY_VALUE',
'Maximum model space distance between geometric entities at asserted c
onnectivities');
#38490=UNCERTAINTY_MEASURE_WITH_UNIT(LENGTH_MEASURE(0.01),#38508,
'DISTANCE_ACCURACY_VALUE',
'Maximum model space distance between geometric entities at asserted c
onnectivities');
#38491=(
GEOMETRIC_REPRESENTATION_CONTEXT(3)
GLOBAL_UNCERTAINTY_ASSIGNED_CONTEXT((#38474))
GLOBAL_UNIT_ASSIGNED_CONTEXT((#38508,#38510,#38511))
REPRESENTATION_CONTEXT('','3D')
);
#38492=(
GEOMETRIC_REPRESENTATION_CONTEXT(3)
GLOBAL_UNCERTAINTY_ASSIGNED_CONTEXT((#38475))
GLOBAL_UNIT_ASSIGNED_CONTEXT((#38508,#38510,#38511))
REPRESENTATION_CONTEXT('','3D')
);
#38493=(
GEOMETRIC_REPRESENTATION_CONTEXT(3)
GLOBAL_UNCERTAINTY_ASSIGNED_CONTEXT((#38476))
GLOBAL_UNIT_ASSIGNED_CONTEXT((#38508,#38510,#38511))
REPRESENTATION_CONTEXT('','3D')
);
#38494=(
GEOMETRIC_REPRESENTATION_CONTEXT(3)
GLOBAL_UNCERTAINTY_ASSIGNED_CONTEXT((#38477))
GLOBAL_UNIT_ASSIGNED_CONTEXT((#38508,#38510,#38511))
REPRESENTATION_CONTEXT('','3D')
);
#38495=(
GEOMETRIC_REPRESENTATION_CONTEXT(3)
GLOBAL_UNCERTAINTY_ASSIGNED_CONTEXT((#38478))
GLOBAL_UNIT_ASSIGNED_CONTEXT((#38508,#38510,#38511))
REPRESENTATION_CONTEXT('','3D')
);
#38496=(
GEOMETRIC_REPRESENTATION_CONTEXT(3)
GLOBAL_UNCERTAINTY_ASSIGNED_CONTEXT((#38479))
GLOBAL_UNIT_ASSIGNED_CONTEXT((#38508,#38510,#38511))
REPRESENTATION_CONTEXT('','3D')
);
#38497=(
GEOMETRIC_REPRESENTATION_CONTEXT(3)
GLOBAL_UNCERTAINTY_ASSIGNED_CONTEXT((#38480))
GLOBAL_UNIT_ASSIGNED_CONTEXT((#38508,#38510,#38511))
REPRESENTATION_CONTEXT('','3D')
);
#38498=(
GEOMETRIC_REPRESENTATION_CONTEXT(3)
GLOBAL_UNCERTAINTY_ASSIGNED_CONTEXT((#38481))
GLOBAL_UNIT_ASSIGNED_CONTEXT((#38508,#38510,#38511))
REPRESENTATION_CONTEXT('','3D')
);
#38499=(
GEOMETRIC_REPRESENTATION_CONTEXT(3)
GLOBAL_UNCERTAINTY_ASSIGNED_CONTEXT((#38482))
GLOBAL_UNIT_ASSIGNED_CONTEXT((#38508,#38510,#38511))
REPRESENTATION_CONTEXT('','3D')
);
#38500=(
GEOMETRIC_REPRESENTATION_CONTEXT(3)
GLOBAL_UNCERTAINTY_ASSIGNED_CONTEXT((#38483))
GLOBAL_UNIT_ASSIGNED_CONTEXT((#38508,#38510,#38511))
REPRESENTATION_CONTEXT('','3D')
);
#38501=(
GEOMETRIC_REPRESENTATION_CONTEXT(3)
GLOBAL_UNCERTAINTY_ASSIGNED_CONTEXT((#38484))
GLOBAL_UNIT_ASSIGNED_CONTEXT((#38508,#38510,#38511))
REPRESENTATION_CONTEXT('','3D')
);
#38502=(
GEOMETRIC_REPRESENTATION_CONTEXT(3)
GLOBAL_UNCERTAINTY_ASSIGNED_CONTEXT((#38485))
GLOBAL_UNIT_ASSIGNED_CONTEXT((#38508,#38510,#38511))
REPRESENTATION_CONTEXT('','3D')
);
#38503=(
GEOMETRIC_REPRESENTATION_CONTEXT(3)
GLOBAL_UNCERTAINTY_ASSIGNED_CONTEXT((#38486))
GLOBAL_UNIT_ASSIGNED_CONTEXT((#38508,#38510,#38511))
REPRESENTATION_CONTEXT('','3D')
);
#38504=(
GEOMETRIC_REPRESENTATION_CONTEXT(3)
GLOBAL_UNCERTAINTY_ASSIGNED_CONTEXT((#38487))
GLOBAL_UNIT_ASSIGNED_CONTEXT((#38508,#38510,#38511))
REPRESENTATION_CONTEXT('','3D')
);
#38505=(
GEOMETRIC_REPRESENTATION_CONTEXT(3)
GLOBAL_UNCERTAINTY_ASSIGNED_CONTEXT((#38488))
GLOBAL_UNIT_ASSIGNED_CONTEXT((#38508,#38510,#38511))
REPRESENTATION_CONTEXT('','3D')
);
#38506=(
GEOMETRIC_REPRESENTATION_CONTEXT(3)
GLOBAL_UNCERTAINTY_ASSIGNED_CONTEXT((#38489))
GLOBAL_UNIT_ASSIGNED_CONTEXT((#38508,#38510,#38511))
REPRESENTATION_CONTEXT('','3D')
);
#38507=(
GEOMETRIC_REPRESENTATION_CONTEXT(3)
GLOBAL_UNCERTAINTY_ASSIGNED_CONTEXT((#38490))
GLOBAL_UNIT_ASSIGNED_CONTEXT((#38508,#38510,#38511))
REPRESENTATION_CONTEXT('','3D')
);
#38508=(
LENGTH_UNIT()
NAMED_UNIT(*)
SI_UNIT(.MILLI.,.METRE.)
);
#38509=(
LENGTH_UNIT()
NAMED_UNIT(*)
SI_UNIT($,.METRE.)
);
#38510=(
NAMED_UNIT(*)
PLANE_ANGLE_UNIT()
SI_UNIT($,.RADIAN.)
);
#38511=(
NAMED_UNIT(*)
SI_UNIT($,.STERADIAN.)
SOLID_ANGLE_UNIT()
);
#38512=SHAPE_DEFINITION_REPRESENTATION(#38528,#38574);
#38513=SHAPE_DEFINITION_REPRESENTATION(#38529,#38575);
#38514=SHAPE_DEFINITION_REPRESENTATION(#38530,#38576);
#38515=SHAPE_DEFINITION_REPRESENTATION(#38531,#38577);
#38516=SHAPE_DEFINITION_REPRESENTATION(#38532,#38578);
#38517=SHAPE_DEFINITION_REPRESENTATION(#38533,#38579);
#38518=SHAPE_DEFINITION_REPRESENTATION(#38534,#38580);
#38519=SHAPE_DEFINITION_REPRESENTATION(#38535,#38581);
#38520=SHAPE_DEFINITION_REPRESENTATION(#38536,#38582);
#38521=SHAPE_DEFINITION_REPRESENTATION(#38537,#38583);
#38522=SHAPE_DEFINITION_REPRESENTATION(#38538,#38584);
#38523=SHAPE_DEFINITION_REPRESENTATION(#38539,#38585);
#38524=SHAPE_DEFINITION_REPRESENTATION(#38540,#38586);
#38525=SHAPE_DEFINITION_REPRESENTATION(#38541,#38587);
#38526=SHAPE_DEFINITION_REPRESENTATION(#38542,#38588);
#38527=SHAPE_DEFINITION_REPRESENTATION(#38543,#38589);
#38528=PRODUCT_DEFINITION_SHAPE('',$,#38591);
#38529=PRODUCT_DEFINITION_SHAPE('',$,#38592);
#38530=PRODUCT_DEFINITION_SHAPE('',$,#38593);
#38531=PRODUCT_DEFINITION_SHAPE('',$,#38594);
#38532=PRODUCT_DEFINITION_SHAPE('',$,#38595);
#38533=PRODUCT_DEFINITION_SHAPE('',$,#38596);
#38534=PRODUCT_DEFINITION_SHAPE('',$,#38597);
#38535=PRODUCT_DEFINITION_SHAPE('',$,#38598);
#38536=PRODUCT_DEFINITION_SHAPE('',$,#38599);
#38537=PRODUCT_DEFINITION_SHAPE('',$,#38600);
#38538=PRODUCT_DEFINITION_SHAPE('',$,#38601);
#38539=PRODUCT_DEFINITION_SHAPE('',$,#38602);
#38540=PRODUCT_DEFINITION_SHAPE('',$,#38603);
#38541=PRODUCT_DEFINITION_SHAPE('',$,#38604);
#38542=PRODUCT_DEFINITION_SHAPE('',$,#38605);
#38543=PRODUCT_DEFINITION_SHAPE('',$,#38606);
#38544=PRODUCT_DEFINITION_SHAPE($,$,#101);
#38545=PRODUCT_DEFINITION_SHAPE($,$,#102);
#38546=PRODUCT_DEFINITION_SHAPE($,$,#103);
#38547=PRODUCT_DEFINITION_SHAPE($,$,#104);
#38548=PRODUCT_DEFINITION_SHAPE($,$,#105);
#38549=PRODUCT_DEFINITION_SHAPE($,$,#106);
#38550=PRODUCT_DEFINITION_SHAPE($,$,#107);
#38551=PRODUCT_DEFINITION_SHAPE($,$,#108);
#38552=PRODUCT_DEFINITION_SHAPE($,$,#109);
#38553=PRODUCT_DEFINITION_SHAPE($,$,#110);
#38554=PRODUCT_DEFINITION_SHAPE($,$,#111);
#38555=PRODUCT_DEFINITION_SHAPE($,$,#112);
#38556=PRODUCT_DEFINITION_SHAPE($,$,#113);
#38557=PRODUCT_DEFINITION_SHAPE($,$,#114);
#38558=PRODUCT_DEFINITION_SHAPE($,$,#115);
#38559=PRODUCT_DEFINITION_SHAPE($,$,#116);
#38560=PRODUCT_DEFINITION_SHAPE($,$,#117);
#38561=PRODUCT_DEFINITION_SHAPE($,$,#118);
#38562=PRODUCT_DEFINITION_SHAPE($,$,#119);
#38563=PRODUCT_DEFINITION_SHAPE($,$,#120);
#38564=PRODUCT_DEFINITION_SHAPE($,$,#121);
#38565=PRODUCT_DEFINITION_SHAPE($,$,#122);
#38566=PRODUCT_DEFINITION_SHAPE($,$,#123);
#38567=PRODUCT_DEFINITION_SHAPE($,$,#124);
#38568=PRODUCT_DEFINITION_SHAPE($,$,#125);
#38569=PRODUCT_DEFINITION_SHAPE($,$,#126);
#38570=PRODUCT_DEFINITION_SHAPE($,$,#127);
#38571=PRODUCT_DEFINITION_SHAPE($,$,#128);
#38572=PRODUCT_DEFINITION_SHAPE($,$,#129);
#38573=PRODUCT_DEFINITION_SHAPE($,$,#130);
#38574=SHAPE_REPRESENTATION('',(#15252,#16745,#16746,#16747,#16748,#16749,
#16750,#16751,#16752,#16753,#16754,#16755,#16756,#16757,#16758,#16759,#16760,
#16761,#16762,#16763,#16764,#16765,#16766,#16767,#16768,#16769,#16770,#16771,
#16772,#16773,#16774),#38491);
#38575=SHAPE_REPRESENTATION('',(#15253),#38492);
#38576=SHAPE_REPRESENTATION('',(#15494),#38493);
#38577=SHAPE_REPRESENTATION('',(#15799),#38494);
#38578=SHAPE_REPRESENTATION('',(#15825),#38495);
#38579=SHAPE_REPRESENTATION('',(#15901),#38496);
#38580=SHAPE_REPRESENTATION('',(#15950),#38497);
#38581=SHAPE_REPRESENTATION('',(#16152),#38498);
#38582=SHAPE_REPRESENTATION('',(#16171),#38499);
#38583=SHAPE_REPRESENTATION('',(#16204),#38500);
#38584=SHAPE_REPRESENTATION('',(#16229),#38501);
#38585=SHAPE_REPRESENTATION('',(#16254),#38502);
#38586=SHAPE_REPRESENTATION('',(#16279),#38503);
#38587=SHAPE_REPRESENTATION('',(#16304),#38504);
#38588=SHAPE_REPRESENTATION('',(#16357),#38505);
#38589=SHAPE_REPRESENTATION('',(#16670),#38506);
#38590=PRODUCT_DEFINITION_CONTEXT('part definition',#38640,'design');
#38591=PRODUCT_DEFINITION('2026-10-26-01-10-33-486','MAS-347',#38607,#38590);
#38592=PRODUCT_DEFINITION('2026-10-26-01-10-34-522',
'01_Housing_SAE_B_Flange',#38608,#38590);
#38593=PRODUCT_DEFINITION('2026-10-26-01-10-37-592',
'02_Port_Plate_Rear_Cap',#38609,#38590);
#38594=PRODUCT_DEFINITION('2026-10-26-01-10-46-042',
'03_Fixed_Swashplate_18deg',#38610,#38590);
#38595=PRODUCT_DEFINITION('2026-10-26-01-10-46-823',
'04_Cylinder_Barrel',#38611,#38590);
#38596=PRODUCT_DEFINITION('2026-10-26-01-10-50-811','08_Valve_Plate',#38612,
#38590);
#38597=PRODUCT_DEFINITION('2026-10-26-01-10-51-970',
'09_Drive_Shaft_SAE_B_13T',#38613,#38590);
#38598=PRODUCT_DEFINITION('2026-10-26-01-10-53-965',
'10_Barrel_Key_DIN_6885_6x6x40',#38614,#38590);
#38599=PRODUCT_DEFINITION('2026-10-26-01-10-54-631',
'11_Front_Bearing_6006',#38615,#38590);
#38600=PRODUCT_DEFINITION('2026-10-26-01-10-55-457',
'12_Rear_Needle_Bearing_NK25-20',#38616,#38590);
#38601=PRODUCT_DEFINITION('2026-10-26-01-10-56-411',
'13_Shaft_Lip_Seal_30x47x7',#38617,#38590);
#38602=PRODUCT_DEFINITION('2026-10-26-01-10-48-079','05_Piston_D17',#38618,
#38590);
#38603=PRODUCT_DEFINITION('2026-10-26-01-10-49-065','06_Slipper_Bronze',
#38619,#38590);
#38604=PRODUCT_DEFINITION('2026-10-26-01-10-50-044',
'07_Slipper_Retainer_Plate',#38620,#38590);
#38605=PRODUCT_DEFINITION('2026-10-26-01-10-57-045',
'14_Cap_Screw_ISO_4762_M12x60',#38621,#38590);
#38606=PRODUCT_DEFINITION('2026-10-26-01-10-59-292',
'15_Drain_Plug_M18x1.5',#38622,#38590);
#38607=PRODUCT_DEFINITION_FORMATION('',$,#38642);
#38608=PRODUCT_DEFINITION_FORMATION('',$,#38643);
#38609=PRODUCT_DEFINITION_FORMATION('',$,#38644);
#38610=PRODUCT_DEFINITION_FORMATION('',$,#38645);
#38611=PRODUCT_DEFINITION_FORMATION('',$,#38646);
#38612=PRODUCT_DEFINITION_FORMATION('',$,#38647);
#38613=PRODUCT_DEFINITION_FORMATION('',$,#38648);
#38614=PRODUCT_DEFINITION_FORMATION('',$,#38649);
#38615=PRODUCT_DEFINITION_FORMATION('',$,#38650);
#38616=PRODUCT_DEFINITION_FORMATION('',$,#38651);
#38617=PRODUCT_DEFINITION_FORMATION('',$,#38652);
#38618=PRODUCT_DEFINITION_FORMATION('',$,#38653);
#38619=PRODUCT_DEFINITION_FORMATION('',$,#38654);
#38620=PRODUCT_DEFINITION_FORMATION('',$,#38655);
#38621=PRODUCT_DEFINITION_FORMATION('',$,#38656);
#38622=PRODUCT_DEFINITION_FORMATION('',$,#38657);
#38623=PRODUCT_RELATED_PRODUCT_CATEGORY('MAS-347','MAS-347',(#38642));
#38624=PRODUCT_RELATED_PRODUCT_CATEGORY('01_Housing_SAE_B_Flange',
'01_Housing_SAE_B_Flange',(#38643));
#38625=PRODUCT_RELATED_PRODUCT_CATEGORY('02_Port_Plate_Rear_Cap',
'02_Port_Plate_Rear_Cap',(#38644));
#38626=PRODUCT_RELATED_PRODUCT_CATEGORY('03_Fixed_Swashplate_18deg',
'03_Fixed_Swashplate_18deg',(#38645));
#38627=PRODUCT_RELATED_PRODUCT_CATEGORY('04_Cylinder_Barrel',
'04_Cylinder_Barrel',(#38646));
#38628=PRODUCT_RELATED_PRODUCT_CATEGORY('08_Valve_Plate',
'08_Valve_Plate',(#38647));
#38629=PRODUCT_RELATED_PRODUCT_CATEGORY('09_Drive_Shaft_SAE_B_13T',
'09_Drive_Shaft_SAE_B_13T',(#38648));
#38630=PRODUCT_RELATED_PRODUCT_CATEGORY('10_Barrel_Key_DIN_6885_6x6x40',
'10_Barrel_Key_DIN_6885_6x6x40',(#38649));
#38631=PRODUCT_RELATED_PRODUCT_CATEGORY('11_Front_Bearing_6006',
'11_Front_Bearing_6006',(#38650));
#38632=PRODUCT_RELATED_PRODUCT_CATEGORY(
'12_Rear_Needle_Bearing_NK25-20','12_Rear_Needle_Bearing_NK25-20',(#38651));
#38633=PRODUCT_RELATED_PRODUCT_CATEGORY('13_Shaft_Lip_Seal_30x47x7',
'13_Shaft_Lip_Seal_30x47x7',(#38652));
#38634=PRODUCT_RELATED_PRODUCT_CATEGORY('05_Piston_D17','05_Piston_D17',
(#38653));
#38635=PRODUCT_RELATED_PRODUCT_CATEGORY('06_Slipper_Bronze',
'06_Slipper_Bronze',(#38654));
#38636=PRODUCT_RELATED_PRODUCT_CATEGORY('07_Slipper_Retainer_Plate',
'07_Slipper_Retainer_Plate',(#38655));
#38637=PRODUCT_RELATED_PRODUCT_CATEGORY('14_Cap_Screw_ISO_4762_M12x60',
'14_Cap_Screw_ISO_4762_M12x60',(#38656));
#38638=PRODUCT_RELATED_PRODUCT_CATEGORY('15_Drain_Plug_M18x1.5',
'15_Drain_Plug_M18x1.5',(#38657));
#38639=APPLICATION_PROTOCOL_DEFINITION('international standard',
'automotive_design',2009,#38640);
#38640=APPLICATION_CONTEXT(
'Core Data for Automotive Mechanical Design Process');
#38641=PRODUCT_CONTEXT('part definition',#38640,'mechanical');
#38642=PRODUCT('2026-10-26-01-10-33-486','MAS-347',$,(#38641));
#38643=PRODUCT('2026-10-26-01-10-34-522','01_Housing_SAE_B_Flange',$,(#38641));
#38644=PRODUCT('2026-10-26-01-10-37-592','02_Port_Plate_Rear_Cap',$,(#38641));
#38645=PRODUCT('2026-10-26-01-10-46-042','03_Fixed_Swashplate_18deg',$,
(#38641));
#38646=PRODUCT('2026-10-26-01-10-46-823','04_Cylinder_Barrel',$,(#38641));
#38647=PRODUCT('2026-10-26-01-10-50-811','08_Valve_Plate',$,(#38641));
#38648=PRODUCT('2026-10-26-01-10-51-970','09_Drive_Shaft_SAE_B_13T',$,(#38641));
#38649=PRODUCT('2026-10-26-01-10-53-965',
'10_Barrel_Key_DIN_6885_6x6x40',$,(#38641));
#38650=PRODUCT('2026-10-26-01-10-54-631','11_Front_Bearing_6006',$,(#38641));
#38651=PRODUCT('2026-10-26-01-10-55-457',
'12_Rear_Needle_Bearing_NK25-20',$,(#38641));
#38652=PRODUCT('2026-10-26-01-10-56-411','13_Shaft_Lip_Seal_30x47x7',$,
(#38641));
#38653=PRODUCT('2026-10-26-01-10-48-079','05_Piston_D17',$,(#38641));
#38654=PRODUCT('2026-10-26-01-10-49-065','06_Slipper_Bronze',$,(#38641));
#38655=PRODUCT('2026-10-26-01-10-50-044','07_Slipper_Retainer_Plate',$,
(#38641));
#38656=PRODUCT('2026-10-26-01-10-57-045','14_Cap_Screw_ISO_4762_M12x60',
$,(#38641));
#38657=PRODUCT('2026-10-26-01-10-59-292','15_Drain_Plug_M18x1.5',$,(#38641));
#38658=PRESENTATION_STYLE_ASSIGNMENT((#38663));
#38659=PRESENTATION_STYLE_ASSIGNMENT((#38664));
#38660=PRESENTATION_STYLE_ASSIGNMENT((#38665));
#38661=PRESENTATION_STYLE_ASSIGNMENT((#38666));
#38662=PRESENTATION_STYLE_ASSIGNMENT((#38667));
#38663=SURFACE_STYLE_USAGE(.BOTH.,#38668);
#38664=SURFACE_STYLE_USAGE(.BOTH.,#38669);
#38665=SURFACE_STYLE_USAGE(.BOTH.,#38670);
#38666=SURFACE_STYLE_USAGE(.BOTH.,#38671);
#38667=SURFACE_STYLE_USAGE(.BOTH.,#38672);
#38668=SURFACE_SIDE_STYLE('',(#38673));
#38669=SURFACE_SIDE_STYLE('',(#38674));
#38670=SURFACE_SIDE_STYLE('',(#38675));
#38671=SURFACE_SIDE_STYLE('',(#38676));
#38672=SURFACE_SIDE_STYLE('',(#38677));
#38673=SURFACE_STYLE_FILL_AREA(#38678);
#38674=SURFACE_STYLE_FILL_AREA(#38679);
#38675=SURFACE_STYLE_FILL_AREA(#38680);
#38676=SURFACE_STYLE_FILL_AREA(#38681);
#38677=SURFACE_STYLE_FILL_AREA(#38682);
#38678=FILL_AREA_STYLE('Steel - Satin',(#38683));
#38679=FILL_AREA_STYLE('MAS496_al',(#38684));
#38680=FILL_AREA_STYLE('MAS496_ti',(#38685));
#38681=FILL_AREA_STYLE('MAS496_ss',(#38686));
#38682=FILL_AREA_STYLE('MAS496_gun',(#38687));
#38683=FILL_AREA_STYLE_COLOUR('Steel - Satin',#38688);
#38684=FILL_AREA_STYLE_COLOUR('MAS496_al',#38689);
#38685=FILL_AREA_STYLE_COLOUR('MAS496_ti',#38690);
#38686=FILL_AREA_STYLE_COLOUR('MAS496_ss',#38691);
#38687=FILL_AREA_STYLE_COLOUR('MAS496_gun',#38692);
#38688=COLOUR_RGB('Steel - Satin',0.627450980392157,0.627450980392157,0.627450980392157);
#38689=COLOUR_RGB('MAS496_al',0.67843137254902,0.705882352941177,0.729411764705882);
#38690=COLOUR_RGB('MAS496_ti',0.549019607843137,0.572549019607843,0.596078431372549);
#38691=COLOUR_RGB('MAS496_ss',0.83921568627451,0.850980392156863,0.862745098039216);
#38692=COLOUR_RGB('MAS496_gun',0.313725490196078,0.337254901960784,0.364705882352941);
#38693=COLOUR_RGB('Dark Blue',0.08,0.2,0.34);
#38694=FILL_AREA_STYLE_COLOUR('',#38693);
#38695=FILL_AREA_STYLE('',(#38694));
#38696=SURFACE_STYLE_FILL_AREA(#38695);
#38697=SURFACE_SIDE_STYLE('',(#38696));
#38698=SURFACE_STYLE_USAGE(.BOTH.,#38697);
#38699=PRESENTATION_STYLE_ASSIGNMENT((#38698));
#38700=COLOUR_RGB('Light Blue',0.38,0.62,0.78);
#38701=FILL_AREA_STYLE_COLOUR('',#38700);
#38702=FILL_AREA_STYLE('',(#38701));
#38703=SURFACE_STYLE_FILL_AREA(#38702);
#38704=SURFACE_SIDE_STYLE('',(#38703));
#38705=SURFACE_STYLE_USAGE(.BOTH.,#38704);
#38706=PRESENTATION_STYLE_ASSIGNMENT((#38705));
#38707=COLOUR_RGB('Sky Blue',0.24,0.69,0.87);
#38708=FILL_AREA_STYLE_COLOUR('',#38707);
#38709=FILL_AREA_STYLE('',(#38708));
#38710=SURFACE_STYLE_FILL_AREA(#38709);
#38711=SURFACE_SIDE_STYLE('',(#38710));
#38712=SURFACE_STYLE_USAGE(.BOTH.,#38711);
#38713=PRESENTATION_STYLE_ASSIGNMENT((#38712));
#38714=COLOUR_RGB('Grey',0.48,0.52,0.57);
#38715=FILL_AREA_STYLE_COLOUR('',#38714);
#38716=FILL_AREA_STYLE('',(#38715));
#38717=SURFACE_STYLE_FILL_AREA(#38716);
#38718=SURFACE_SIDE_STYLE('',(#38717));
#38719=SURFACE_STYLE_USAGE(.BOTH.,#38718);
#38720=PRESENTATION_STYLE_ASSIGNMENT((#38719));
#38721=COLOUR_RGB('Black',0.12,0.14,0.17);
#38722=FILL_AREA_STYLE_COLOUR('',#38721);
#38723=FILL_AREA_STYLE('',(#38722));
#38724=SURFACE_STYLE_FILL_AREA(#38723);
#38725=SURFACE_SIDE_STYLE('',(#38724));
#38726=SURFACE_STYLE_USAGE(.BOTH.,#38725);
#38727=PRESENTATION_STYLE_ASSIGNMENT((#38726));
#38728=COLOUR_RGB('Off White',0.89,0.88,0.83);
#38729=FILL_AREA_STYLE_COLOUR('',#38728);
#38730=FILL_AREA_STYLE('',(#38729));
#38731=SURFACE_STYLE_FILL_AREA(#38730);
#38732=SURFACE_SIDE_STYLE('',(#38731));
#38733=SURFACE_STYLE_USAGE(.BOTH.,#38732);
#38734=PRESENTATION_STYLE_ASSIGNMENT((#38733));
ENDSEC;
END-ISO-10303-21;
